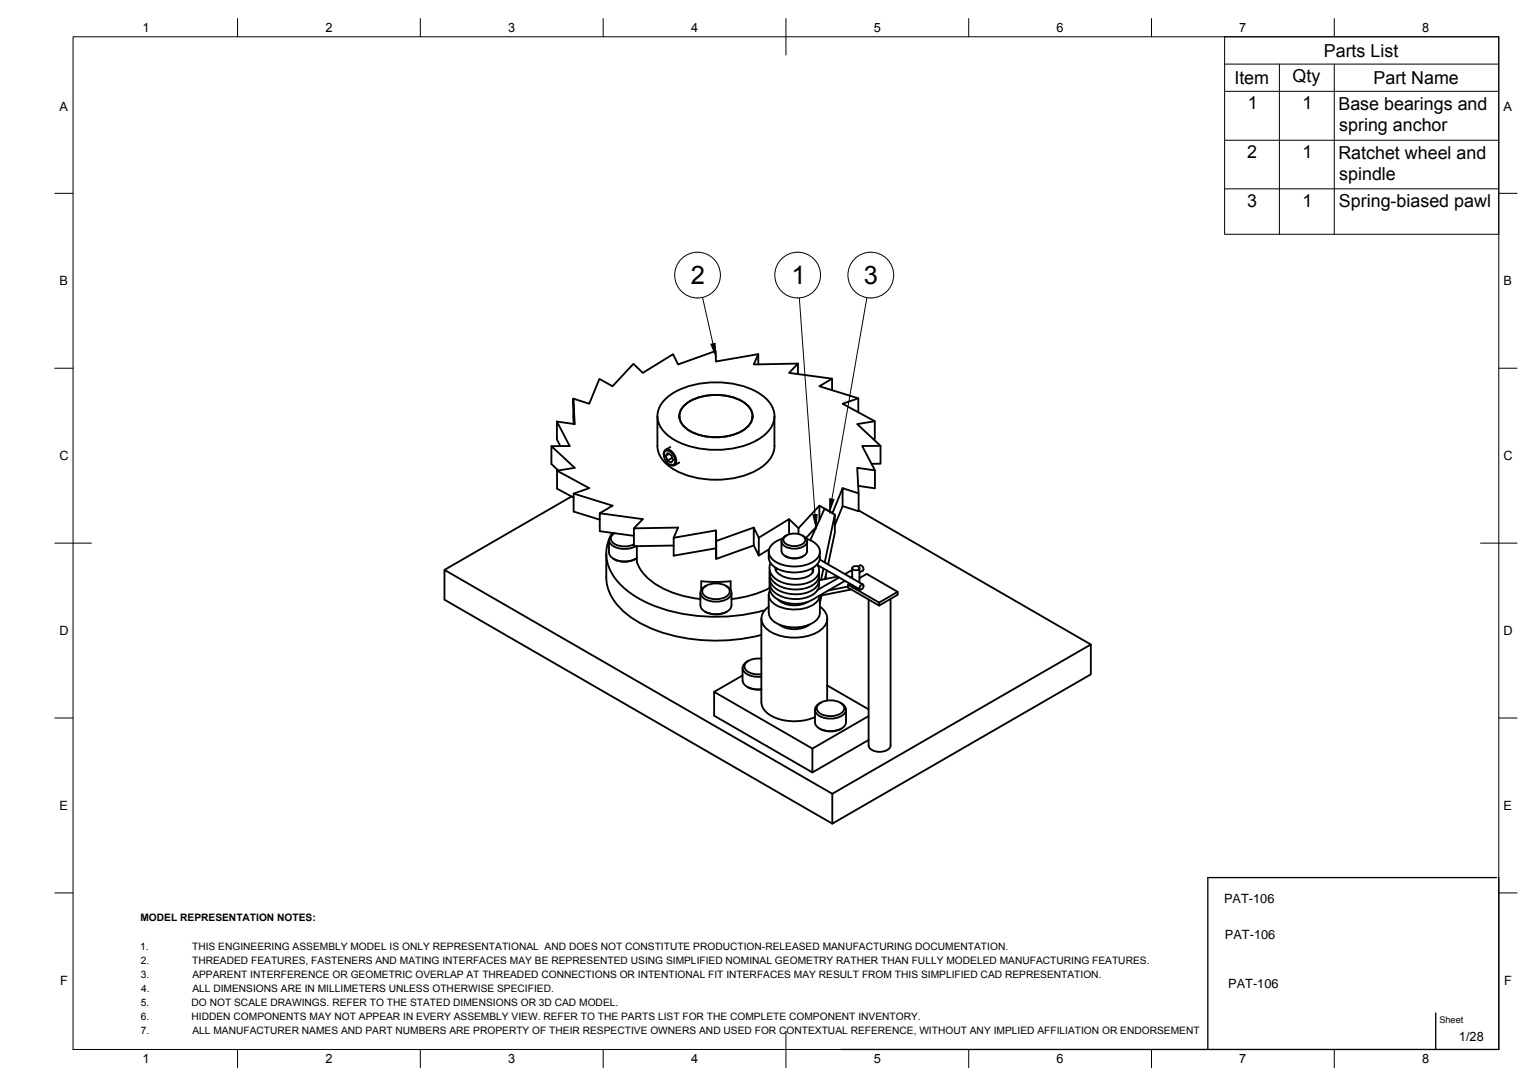
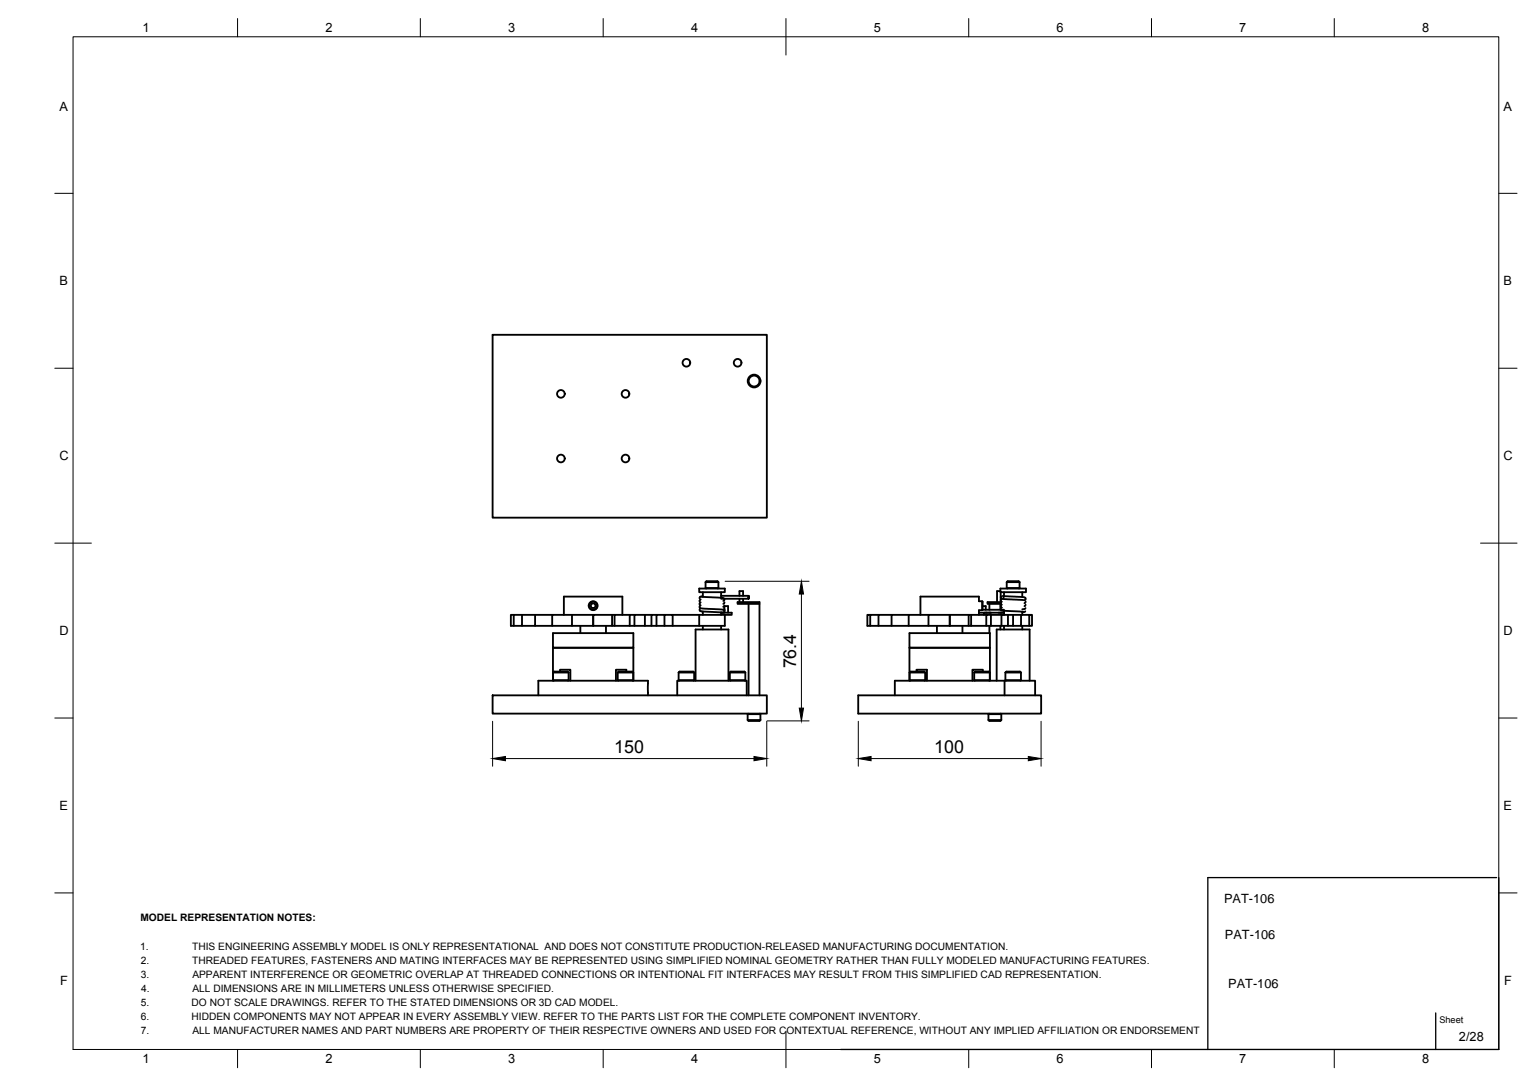
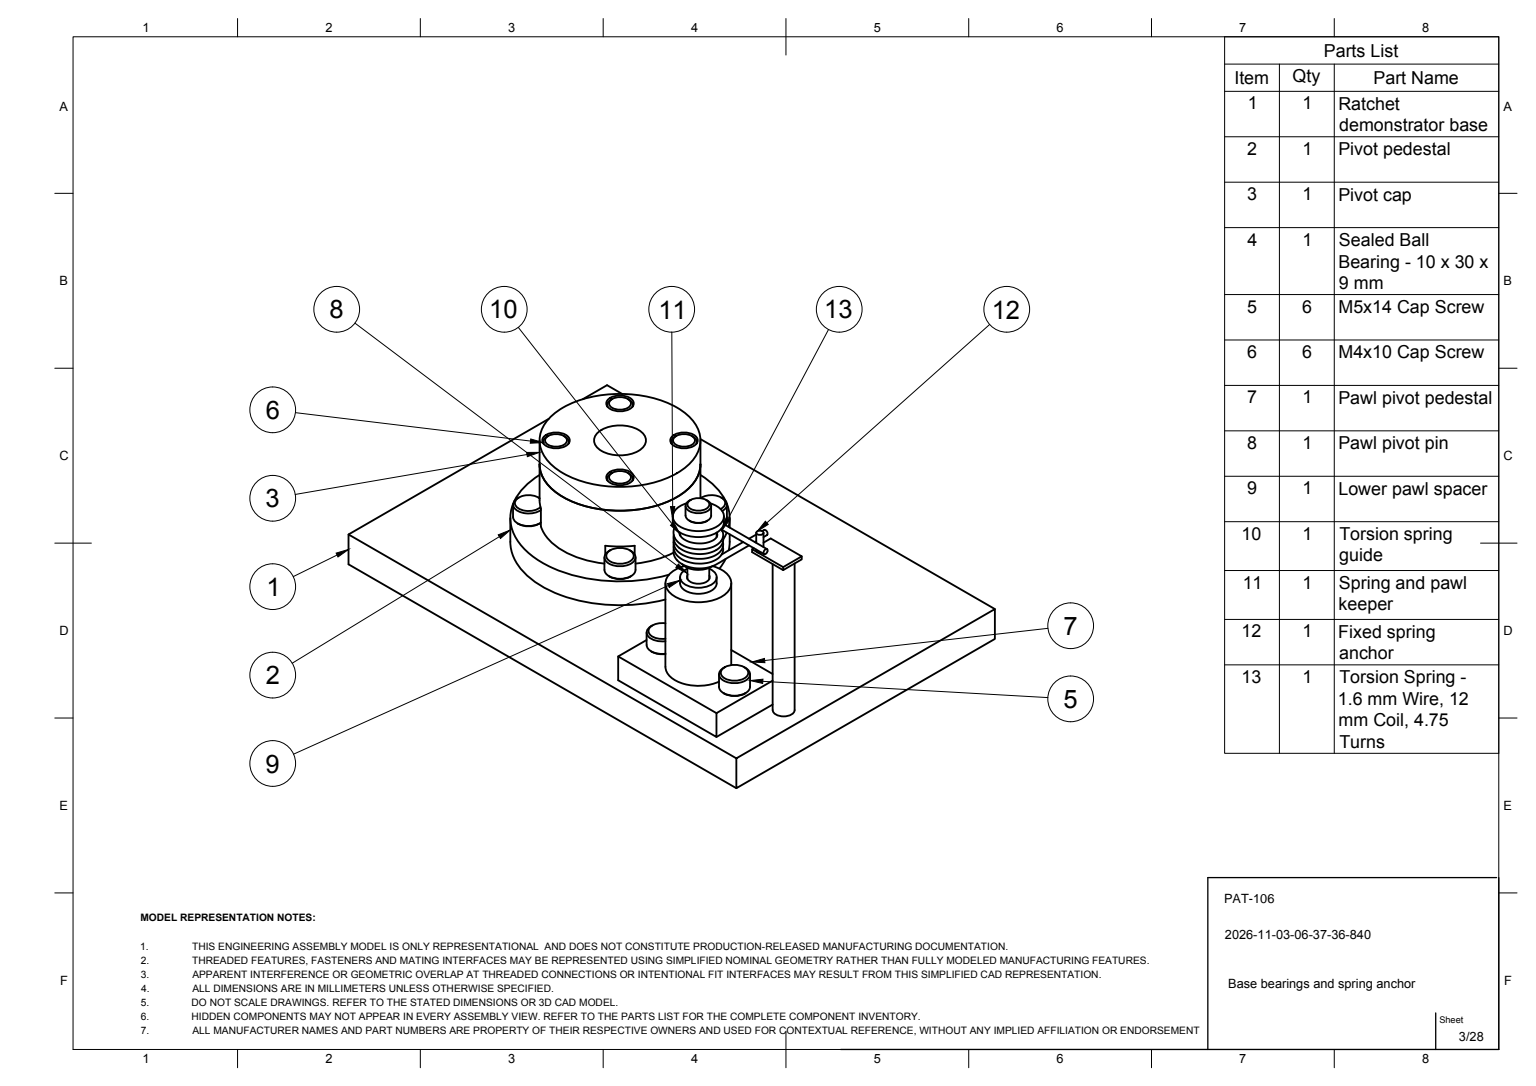
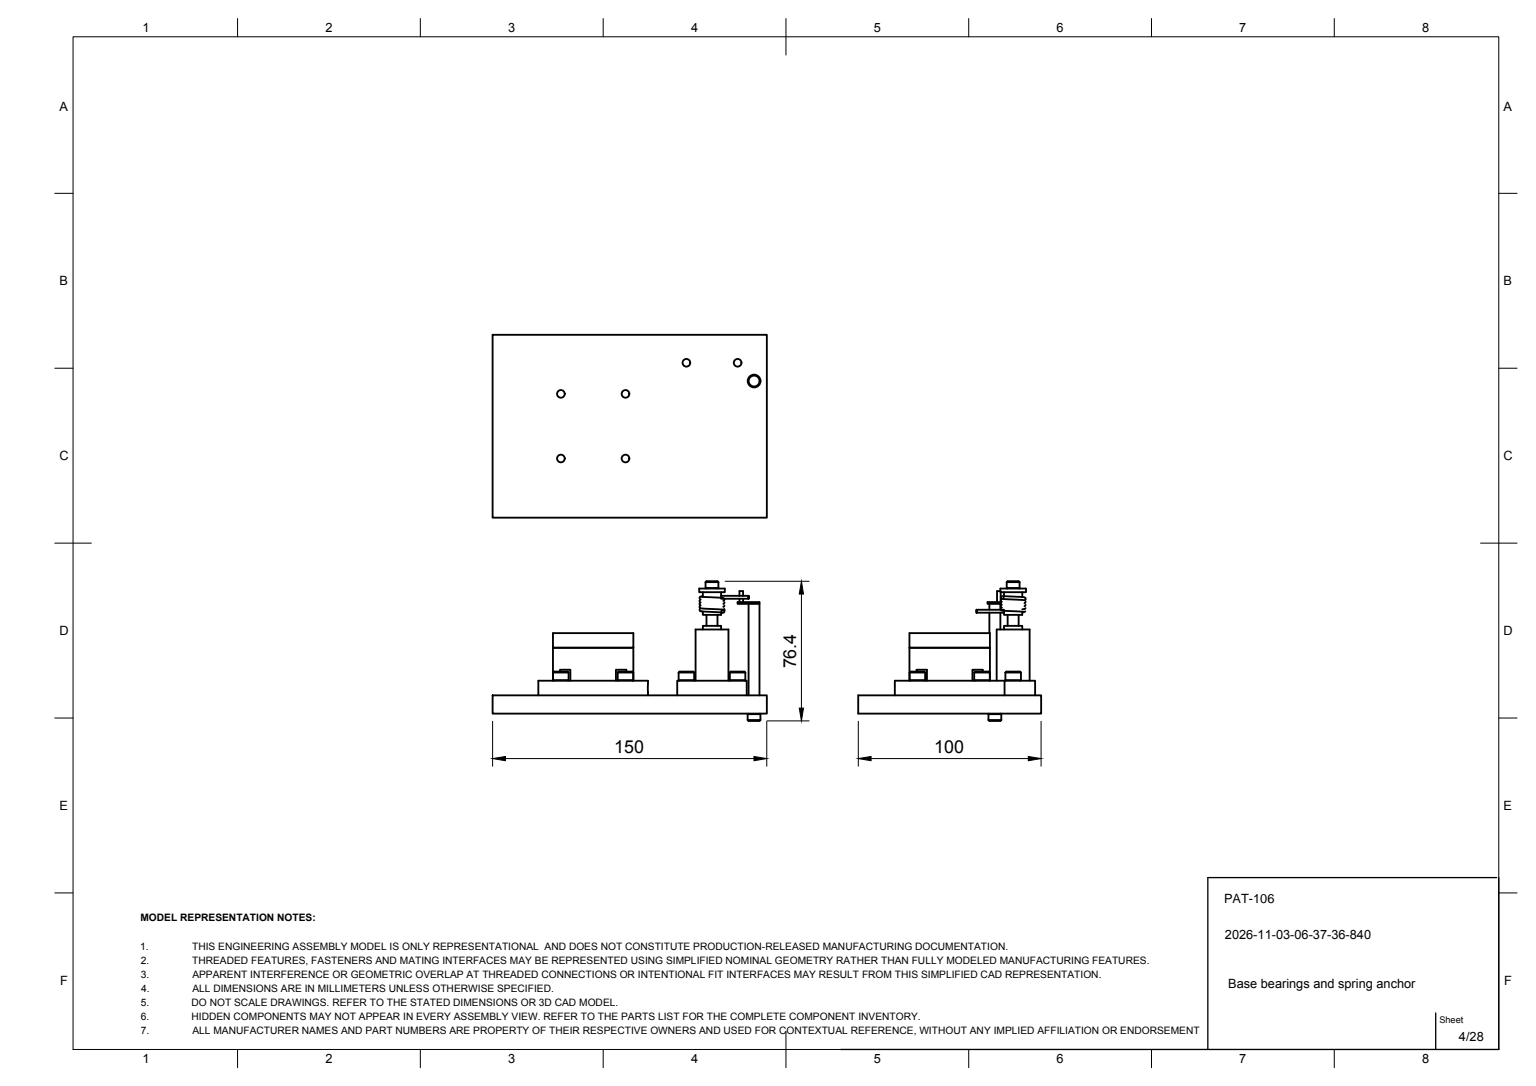
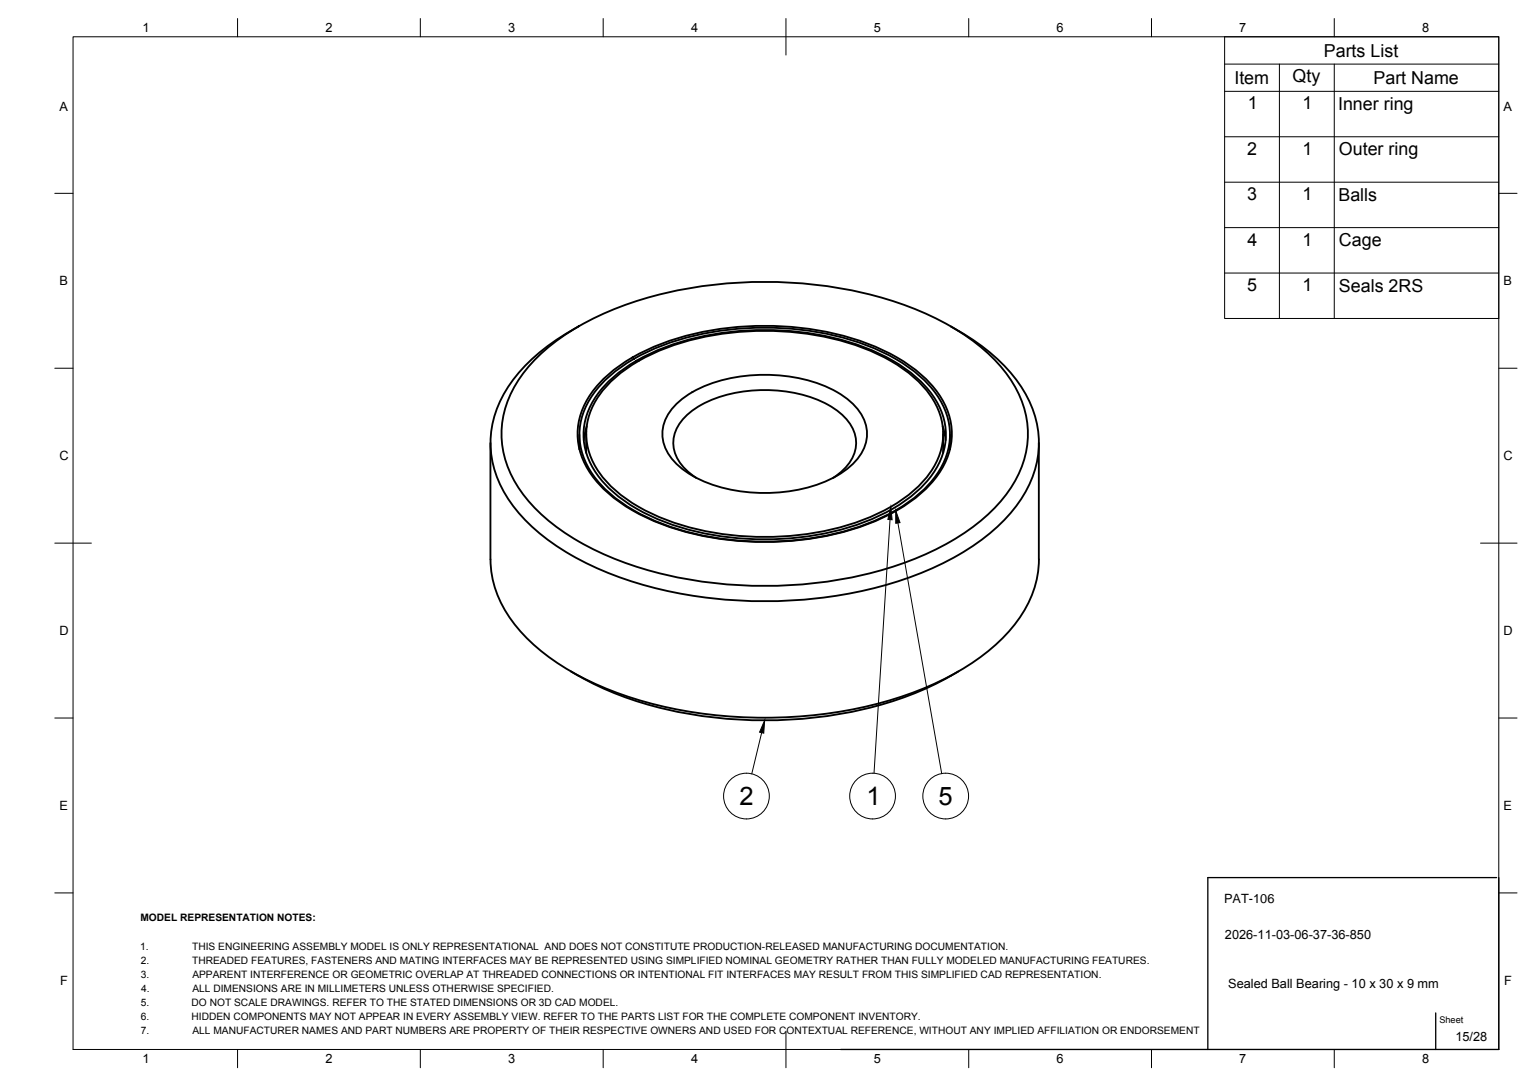
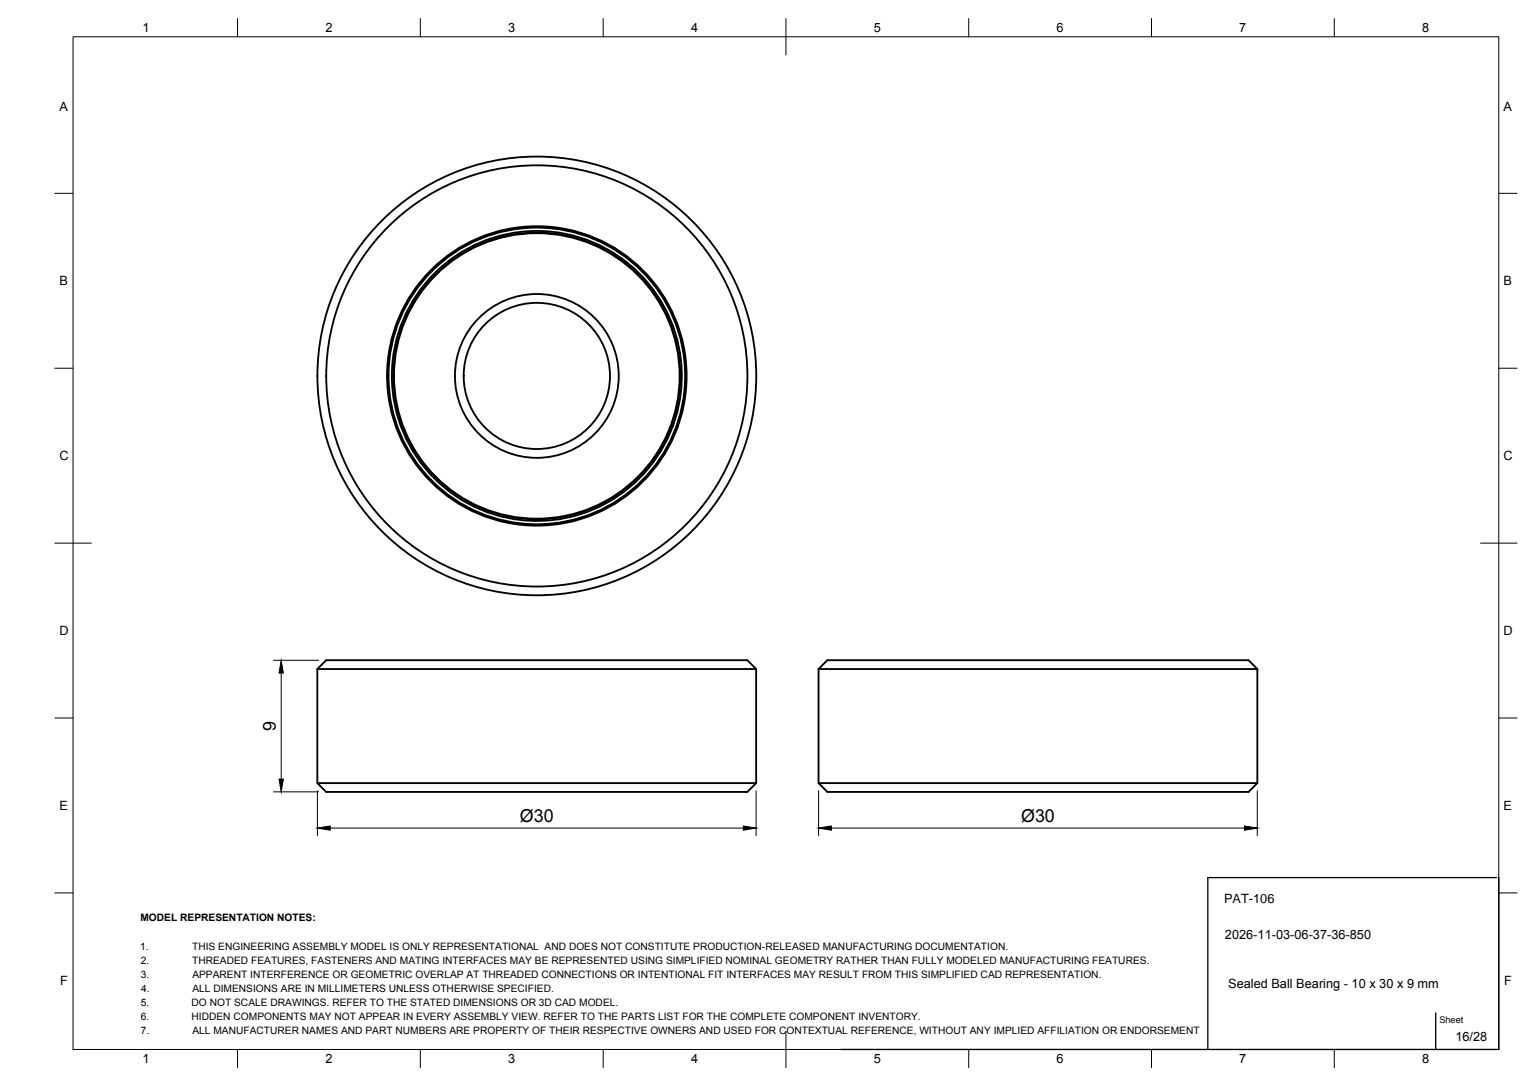
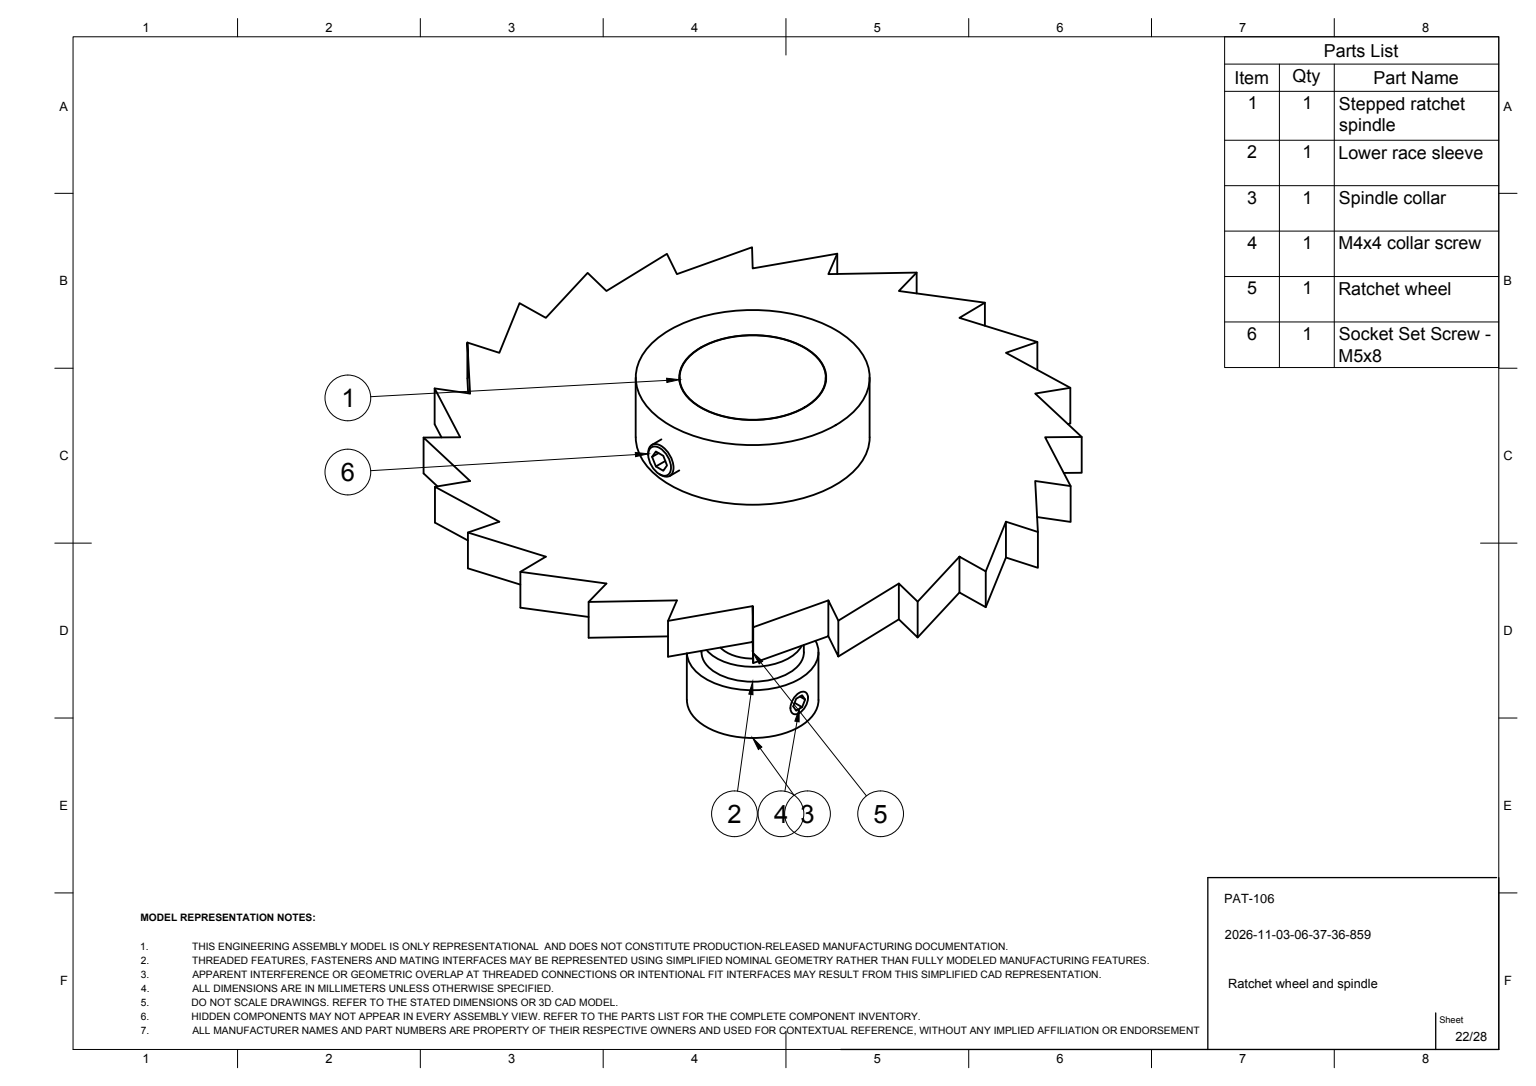
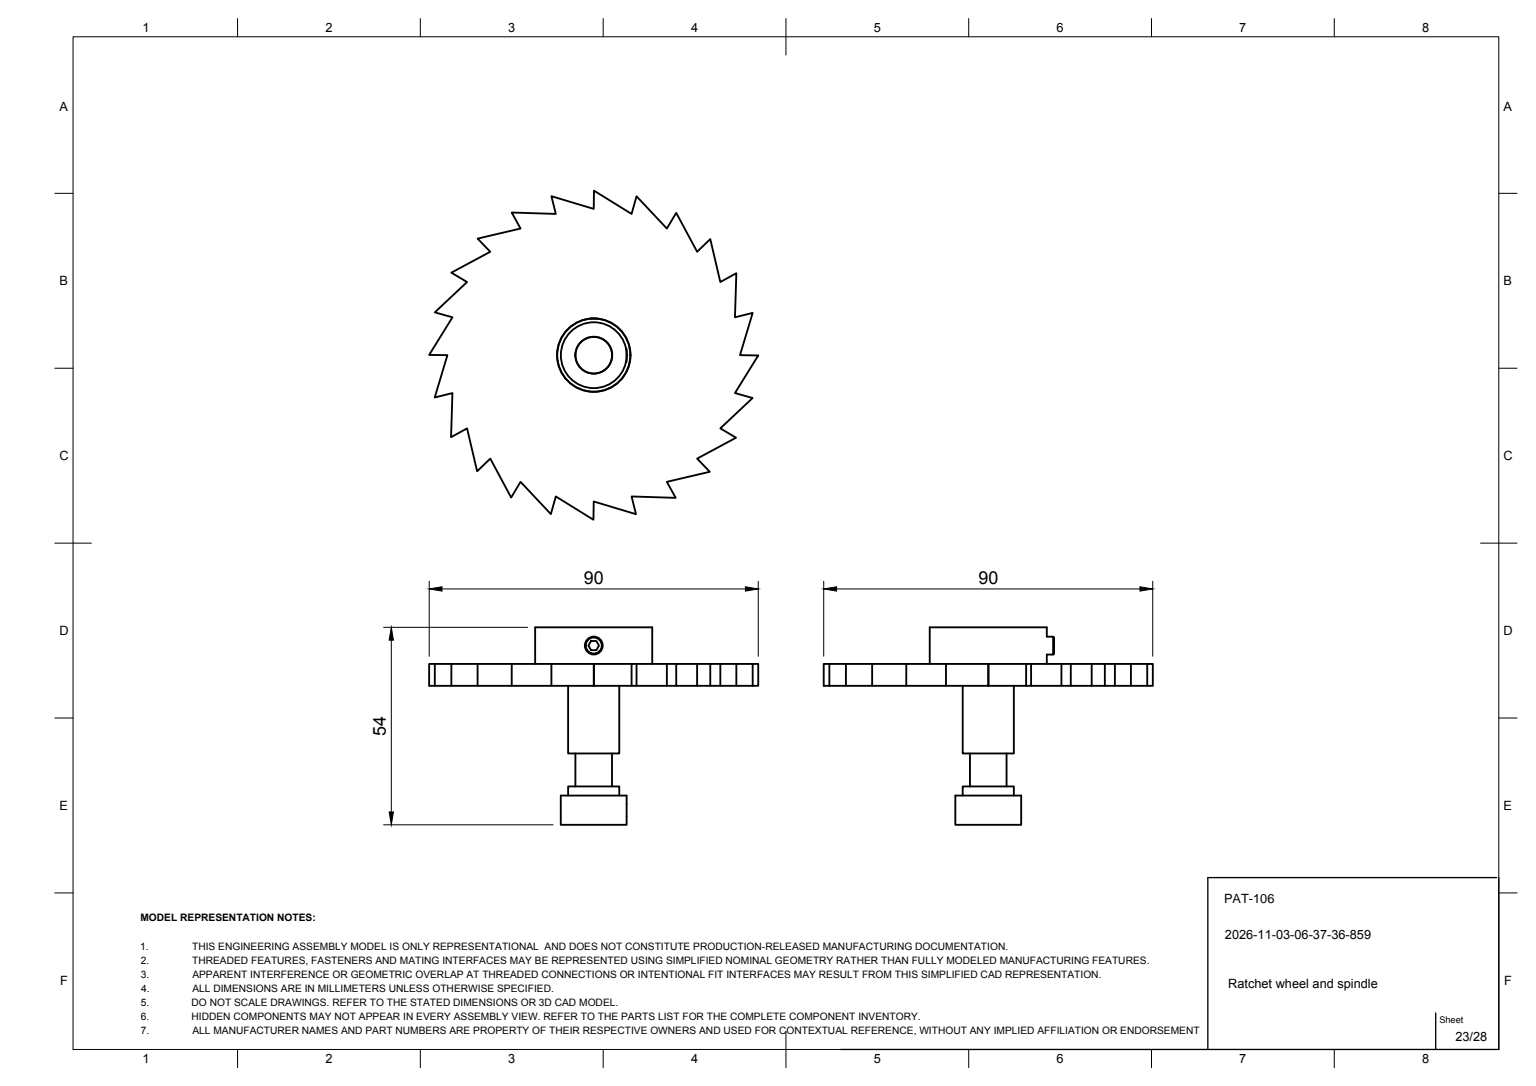
ISO-10303-21;
HEADER;
/* Generated by software containing ST-Developer
 * from STEP Tools, Inc. (www.steptools.com) 
 */

FILE_DESCRIPTION(
/* description */ ('Torsion-spring ratchet demonstrator'),
/* implementation_level */ '2;1');

FILE_NAME(
/* name */ 'PAT-106',
/* time_stamp */ '2026-10-29T17:29:17-07:00',
/* author */ (''),
/* organization */ (''),
/* preprocessor_version */ 'ST-DEVELOPER v20.2',
/* originating_system */ 'Autodesk Translation Framework v15.17.0.0',
/* authorisation */ '');

FILE_SCHEMA (('AUTOMOTIVE_DESIGN { 1 0 10303 214 3 1 1 }'));
ENDSEC;

DATA;
#10=MECHANICAL_DESIGN_GEOMETRIC_PRESENTATION_REPRESENTATION('',(#283,#284,
#285,#286,#287,#288,#289,#290,#291,#292,#293,#294,#295,#296,#297,#298,#299,
#300,#301,#302,#303,#304,#305,#306,#307,#308,#309,#310,#311,#312,#313,#314),
#11258);
#11=B_SPLINE_SURFACE_WITH_KNOTS('',3,3,((#8927,#8928,#8929,#8930,#8931,
#8932,#8933,#8934,#8935,#8936,#8937,#8938,#8939,#8940,#8941,#8942,#8943,
#8944,#8945,#8946,#8947,#8948,#8949,#8950,#8951,#8952,#8953,#8954,#8955,
#8956,#8957,#8958,#8959,#8960,#8961,#8962,#8963,#8964,#8965,#8966,#8967,
#8968,#8969,#8970,#8971,#8972,#8973,#8974,#8975,#8976,#8977,#8978,#8979,
#8980,#8981,#8982,#8983,#8984,#8985,#8986,#8987,#8988,#8989,#8990,#8991,
#8992,#8993),(#8994,#8995,#8996,#8997,#8998,#8999,#9000,#9001,#9002,#9003,
#9004,#9005,#9006,#9007,#9008,#9009,#9010,#9011,#9012,#9013,#9014,#9015,
#9016,#9017,#9018,#9019,#9020,#9021,#9022,#9023,#9024,#9025,#9026,#9027,
#9028,#9029,#9030,#9031,#9032,#9033,#9034,#9035,#9036,#9037,#9038,#9039,
#9040,#9041,#9042,#9043,#9044,#9045,#9046,#9047,#9048,#9049,#9050,#9051,
#9052,#9053,#9054,#9055,#9056,#9057,#9058,#9059,#9060),(#9061,#9062,#9063,
#9064,#9065,#9066,#9067,#9068,#9069,#9070,#9071,#9072,#9073,#9074,#9075,
#9076,#9077,#9078,#9079,#9080,#9081,#9082,#9083,#9084,#9085,#9086,#9087,
#9088,#9089,#9090,#9091,#9092,#9093,#9094,#9095,#9096,#9097,#9098,#9099,
#9100,#9101,#9102,#9103,#9104,#9105,#9106,#9107,#9108,#9109,#9110,#9111,
#9112,#9113,#9114,#9115,#9116,#9117,#9118,#9119,#9120,#9121,#9122,#9123,
#9124,#9125,#9126,#9127),(#9128,#9129,#9130,#9131,#9132,#9133,#9134,#9135,
#9136,#9137,#9138,#9139,#9140,#9141,#9142,#9143,#9144,#9145,#9146,#9147,
#9148,#9149,#9150,#9151,#9152,#9153,#9154,#9155,#9156,#9157,#9158,#9159,
#9160,#9161,#9162,#9163,#9164,#9165,#9166,#9167,#9168,#9169,#9170,#9171,
#9172,#9173,#9174,#9175,#9176,#9177,#9178,#9179,#9180,#9181,#9182,#9183,
#9184,#9185,#9186,#9187,#9188,#9189,#9190,#9191,#9192,#9193,#9194),(#9195,
#9196,#9197,#9198,#9199,#9200,#9201,#9202,#9203,#9204,#9205,#9206,#9207,
#9208,#9209,#9210,#9211,#9212,#9213,#9214,#9215,#9216,#9217,#9218,#9219,
#9220,#9221,#9222,#9223,#9224,#9225,#9226,#9227,#9228,#9229,#9230,#9231,
#9232,#9233,#9234,#9235,#9236,#9237,#9238,#9239,#9240,#9241,#9242,#9243,
#9244,#9245,#9246,#9247,#9248,#9249,#9250,#9251,#9252,#9253,#9254,#9255,
#9256,#9257,#9258,#9259,#9260,#9261),(#9262,#9263,#9264,#9265,#9266,#9267,
#9268,#9269,#9270,#9271,#9272,#9273,#9274,#9275,#9276,#9277,#9278,#9279,
#9280,#9281,#9282,#9283,#9284,#9285,#9286,#9287,#9288,#9289,#9290,#9291,
#9292,#9293,#9294,#9295,#9296,#9297,#9298,#9299,#9300,#9301,#9302,#9303,
#9304,#9305,#9306,#9307,#9308,#9309,#9310,#9311,#9312,#9313,#9314,#9315,
#9316,#9317,#9318,#9319,#9320,#9321,#9322,#9323,#9324,#9325,#9326,#9327,
#9328),(#9329,#9330,#9331,#9332,#9333,#9334,#9335,#9336,#9337,#9338,#9339,
#9340,#9341,#9342,#9343,#9344,#9345,#9346,#9347,#9348,#9349,#9350,#9351,
#9352,#9353,#9354,#9355,#9356,#9357,#9358,#9359,#9360,#9361,#9362,#9363,
#9364,#9365,#9366,#9367,#9368,#9369,#9370,#9371,#9372,#9373,#9374,#9375,
#9376,#9377,#9378,#9379,#9380,#9381,#9382,#9383,#9384,#9385,#9386,#9387,
#9388,#9389,#9390,#9391,#9392,#9393,#9394,#9395),(#9396,#9397,#9398,#9399,
#9400,#9401,#9402,#9403,#9404,#9405,#9406,#9407,#9408,#9409,#9410,#9411,
#9412,#9413,#9414,#9415,#9416,#9417,#9418,#9419,#9420,#9421,#9422,#9423,
#9424,#9425,#9426,#9427,#9428,#9429,#9430,#9431,#9432,#9433,#9434,#9435,
#9436,#9437,#9438,#9439,#9440,#9441,#9442,#9443,#9444,#9445,#9446,#9447,
#9448,#9449,#9450,#9451,#9452,#9453,#9454,#9455,#9456,#9457,#9458,#9459,
#9460,#9461,#9462),(#9463,#9464,#9465,#9466,#9467,#9468,#9469,#9470,#9471,
#9472,#9473,#9474,#9475,#9476,#9477,#9478,#9479,#9480,#9481,#9482,#9483,
#9484,#9485,#9486,#9487,#9488,#9489,#9490,#9491,#9492,#9493,#9494,#9495,
#9496,#9497,#9498,#9499,#9500,#9501,#9502,#9503,#9504,#9505,#9506,#9507,
#9508,#9509,#9510,#9511,#9512,#9513,#9514,#9515,#9516,#9517,#9518,#9519,
#9520,#9521,#9522,#9523,#9524,#9525,#9526,#9527,#9528,#9529)),
 .UNSPECIFIED.,.F.,.F.,.F.,(4,1,1,1,1,1,4),(4,1,1,1,1,1,1,1,1,1,1,1,1,1,
1,1,1,1,1,1,1,1,1,1,1,1,1,1,1,1,1,1,1,1,1,1,1,1,1,1,1,1,1,1,1,1,1,1,1,1,
1,1,1,1,1,1,1,1,1,1,1,1,1,1,4),(-2.2472005777546,-1.52802098913967,-0.808841400524738,
-0.329388341448117,0.150064717628504,0.629517776705124,1.10897083578174),
(0.,0.0178571428571429,0.0357142857142857,0.0446428571428571,0.0535714285714286,
0.0625,0.0714285714285714,0.0803571428571428,0.0848214285714286,0.0892857142857143,
0.0982142857142857,0.107142857142857,0.125,0.142857142857143,0.166666666666667,
0.19047619047619,0.214285714285714,0.232142857142857,0.25,0.267857142857143,
0.285714285714286,0.303571428571429,0.321428571428571,0.339285714285714,
0.357142857142857,0.369047619047619,0.392857142857143,0.410714285714286,
0.428571428571429,0.452380952380952,0.476190476190476,0.492063492063492,
0.507936507936508,0.523809523809524,0.547619047619048,0.571428571428571,
0.595238095238095,0.619047619047619,0.642857142857143,0.666666666666667,
0.682539682539682,0.698412698412698,0.714285714285714,0.73015873015873,
0.746031746031746,0.761904761904762,0.785714285714286,0.809523809523809,
0.833333333333333,0.857142857142857,0.861607142857143,0.866071428571429,
0.875,0.892857142857143,0.901785714285714,0.910714285714286,0.915178571428571,
0.919642857142857,0.928571428571429,0.9375,0.946428571428571,0.955357142857143,
0.964285714285714,0.982142857142857,1.),.UNSPECIFIED.);
#12=B_SPLINE_SURFACE_WITH_KNOTS('',3,3,((#9670,#9671,#9672,#9673,#9674,
#9675,#9676,#9677,#9678,#9679,#9680,#9681,#9682,#9683,#9684,#9685,#9686,
#9687,#9688,#9689,#9690,#9691,#9692,#9693,#9694,#9695,#9696,#9697,#9698,
#9699,#9700,#9701,#9702,#9703,#9704,#9705,#9706,#9707,#9708,#9709,#9710,
#9711,#9712,#9713,#9714,#9715,#9716,#9717,#9718,#9719,#9720,#9721,#9722,
#9723,#9724,#9725,#9726,#9727,#9728,#9729,#9730,#9731,#9732,#9733,#9734,
#9735,#9736,#9737,#9738,#9739,#9740),(#9741,#9742,#9743,#9744,#9745,#9746,
#9747,#9748,#9749,#9750,#9751,#9752,#9753,#9754,#9755,#9756,#9757,#9758,
#9759,#9760,#9761,#9762,#9763,#9764,#9765,#9766,#9767,#9768,#9769,#9770,
#9771,#9772,#9773,#9774,#9775,#9776,#9777,#9778,#9779,#9780,#9781,#9782,
#9783,#9784,#9785,#9786,#9787,#9788,#9789,#9790,#9791,#9792,#9793,#9794,
#9795,#9796,#9797,#9798,#9799,#9800,#9801,#9802,#9803,#9804,#9805,#9806,
#9807,#9808,#9809,#9810,#9811),(#9812,#9813,#9814,#9815,#9816,#9817,#9818,
#9819,#9820,#9821,#9822,#9823,#9824,#9825,#9826,#9827,#9828,#9829,#9830,
#9831,#9832,#9833,#9834,#9835,#9836,#9837,#9838,#9839,#9840,#9841,#9842,
#9843,#9844,#9845,#9846,#9847,#9848,#9849,#9850,#9851,#9852,#9853,#9854,
#9855,#9856,#9857,#9858,#9859,#9860,#9861,#9862,#9863,#9864,#9865,#9866,
#9867,#9868,#9869,#9870,#9871,#9872,#9873,#9874,#9875,#9876,#9877,#9878,
#9879,#9880,#9881,#9882),(#9883,#9884,#9885,#9886,#9887,#9888,#9889,#9890,
#9891,#9892,#9893,#9894,#9895,#9896,#9897,#9898,#9899,#9900,#9901,#9902,
#9903,#9904,#9905,#9906,#9907,#9908,#9909,#9910,#9911,#9912,#9913,#9914,
#9915,#9916,#9917,#9918,#9919,#9920,#9921,#9922,#9923,#9924,#9925,#9926,
#9927,#9928,#9929,#9930,#9931,#9932,#9933,#9934,#9935,#9936,#9937,#9938,
#9939,#9940,#9941,#9942,#9943,#9944,#9945,#9946,#9947,#9948,#9949,#9950,
#9951,#9952,#9953)),.UNSPECIFIED.,.F.,.F.,.F.,(4,4),(4,1,1,1,1,1,1,1,1,
1,1,1,1,1,1,1,1,1,1,1,1,1,1,1,1,1,1,1,1,1,1,1,1,1,1,1,1,1,1,1,1,1,1,1,1,
1,1,1,1,1,1,1,1,1,1,1,1,1,1,1,1,1,1,1,1,1,1,1,4),(3.14159265358979,4.03598472942499),
(0.,0.0178571428571429,0.0357142857142857,0.0446428571428571,0.0535714285714286,
0.0625,0.0714285714285714,0.0803571428571428,0.0892857142857143,0.0982142857142857,
0.107142857142857,0.125,0.142857142857143,0.166666666666667,0.19047619047619,
0.196428571428571,0.214285714285714,0.232142857142857,0.25,0.267857142857143,
0.285714285714286,0.303571428571429,0.321428571428571,0.339285714285714,
0.357142857142857,0.369047619047619,0.392857142857143,0.410714285714286,
0.419642857142857,0.428571428571429,0.452380952380952,0.476190476190476,
0.492063492063492,0.5,0.507936507936508,0.523809523809524,0.547619047619048,
0.571428571428571,0.595238095238095,0.619047619047619,0.642857142857143,
0.666666666666667,0.682539682539682,0.698412698412698,0.714285714285714,
0.722222222222222,0.73015873015873,0.746031746031746,0.761904761904762,
0.773809523809524,0.785714285714286,0.809523809523809,0.833333333333333,
0.857142857142857,0.859375,0.861607142857143,0.866071428571429,0.875,0.892857142857143,
0.901785714285714,0.910714285714286,0.919642857142857,0.928571428571429,
0.9375,0.946428571428571,0.955357142857143,0.964285714285714,0.982142857142857,
1.),.UNSPECIFIED.);
#13=B_SPLINE_SURFACE_WITH_KNOTS('',3,3,((#10029,#10030,#10031,#10032,#10033,
#10034,#10035,#10036,#10037,#10038,#10039,#10040,#10041,#10042,#10043,#10044,
#10045,#10046,#10047,#10048,#10049,#10050,#10051,#10052,#10053,#10054,#10055,
#10056,#10057,#10058,#10059,#10060,#10061,#10062,#10063,#10064,#10065,#10066,
#10067,#10068,#10069,#10070,#10071,#10072,#10073,#10074,#10075,#10076,#10077,
#10078,#10079,#10080,#10081,#10082,#10083,#10084,#10085,#10086,#10087,#10088,
#10089,#10090,#10091,#10092,#10093,#10094,#10095,#10096,#10097,#10098,#10099,
#10100),(#10101,#10102,#10103,#10104,#10105,#10106,#10107,#10108,#10109,
#10110,#10111,#10112,#10113,#10114,#10115,#10116,#10117,#10118,#10119,#10120,
#10121,#10122,#10123,#10124,#10125,#10126,#10127,#10128,#10129,#10130,#10131,
#10132,#10133,#10134,#10135,#10136,#10137,#10138,#10139,#10140,#10141,#10142,
#10143,#10144,#10145,#10146,#10147,#10148,#10149,#10150,#10151,#10152,#10153,
#10154,#10155,#10156,#10157,#10158,#10159,#10160,#10161,#10162,#10163,#10164,
#10165,#10166,#10167,#10168,#10169,#10170,#10171,#10172),(#10173,#10174,
#10175,#10176,#10177,#10178,#10179,#10180,#10181,#10182,#10183,#10184,#10185,
#10186,#10187,#10188,#10189,#10190,#10191,#10192,#10193,#10194,#10195,#10196,
#10197,#10198,#10199,#10200,#10201,#10202,#10203,#10204,#10205,#10206,#10207,
#10208,#10209,#10210,#10211,#10212,#10213,#10214,#10215,#10216,#10217,#10218,
#10219,#10220,#10221,#10222,#10223,#10224,#10225,#10226,#10227,#10228,#10229,
#10230,#10231,#10232,#10233,#10234,#10235,#10236,#10237,#10238,#10239,#10240,
#10241,#10242,#10243,#10244),(#10245,#10246,#10247,#10248,#10249,#10250,
#10251,#10252,#10253,#10254,#10255,#10256,#10257,#10258,#10259,#10260,#10261,
#10262,#10263,#10264,#10265,#10266,#10267,#10268,#10269,#10270,#10271,#10272,
#10273,#10274,#10275,#10276,#10277,#10278,#10279,#10280,#10281,#10282,#10283,
#10284,#10285,#10286,#10287,#10288,#10289,#10290,#10291,#10292,#10293,#10294,
#10295,#10296,#10297,#10298,#10299,#10300,#10301,#10302,#10303,#10304,#10305,
#10306,#10307,#10308,#10309,#10310,#10311,#10312,#10313,#10314,#10315,#10316),
(#10317,#10318,#10319,#10320,#10321,#10322,#10323,#10324,#10325,#10326,
#10327,#10328,#10329,#10330,#10331,#10332,#10333,#10334,#10335,#10336,#10337,
#10338,#10339,#10340,#10341,#10342,#10343,#10344,#10345,#10346,#10347,#10348,
#10349,#10350,#10351,#10352,#10353,#10354,#10355,#10356,#10357,#10358,#10359,
#10360,#10361,#10362,#10363,#10364,#10365,#10366,#10367,#10368,#10369,#10370,
#10371,#10372,#10373,#10374,#10375,#10376,#10377,#10378,#10379,#10380,#10381,
#10382,#10383,#10384,#10385,#10386,#10387,#10388),(#10389,#10390,#10391,
#10392,#10393,#10394,#10395,#10396,#10397,#10398,#10399,#10400,#10401,#10402,
#10403,#10404,#10405,#10406,#10407,#10408,#10409,#10410,#10411,#10412,#10413,
#10414,#10415,#10416,#10417,#10418,#10419,#10420,#10421,#10422,#10423,#10424,
#10425,#10426,#10427,#10428,#10429,#10430,#10431,#10432,#10433,#10434,#10435,
#10436,#10437,#10438,#10439,#10440,#10441,#10442,#10443,#10444,#10445,#10446,
#10447,#10448,#10449,#10450,#10451,#10452,#10453,#10454,#10455,#10456,#10457,
#10458,#10459,#10460)),.UNSPECIFIED.,.F.,.F.,.F.,(4,1,1,4),(4,1,1,1,1,1,
1,1,1,1,1,1,1,1,1,1,1,1,1,1,1,1,1,1,1,1,1,1,1,1,1,1,1,1,1,1,1,1,1,1,1,1,
1,1,1,1,1,1,1,1,1,1,1,1,1,1,1,1,1,1,1,1,1,1,1,1,1,1,1,4),(1.10897083578174,
1.98009447198525,2.56084356278759,3.14159265358993),(0.,0.0178571428571429,
0.0357142857142857,0.0446428571428571,0.0535714285714286,0.0625,0.0714285714285714,
0.0803571428571428,0.0848214285714286,0.0892857142857143,0.0982142857142857,
0.107142857142857,0.125,0.142857142857143,0.166666666666667,0.19047619047619,
0.196428571428571,0.214285714285714,0.232142857142857,0.25,0.267857142857143,
0.285714285714286,0.303571428571429,0.321428571428571,0.339285714285714,
0.357142857142857,0.369047619047619,0.392857142857143,0.410714285714286,
0.419642857142857,0.428571428571429,0.452380952380952,0.476190476190476,
0.492063492063492,0.507936507936508,0.523809523809524,0.547619047619048,
0.571428571428571,0.595238095238095,0.619047619047619,0.642857142857143,
0.666666666666667,0.682539682539682,0.698412698412698,0.714285714285714,
0.73015873015873,0.746031746031746,0.761904761904762,0.773809523809524,
0.785714285714286,0.791666666666667,0.809523809523809,0.833333333333333,
0.857142857142857,0.859375,0.861607142857143,0.866071428571429,0.875,0.892857142857143,
0.901785714285714,0.910714285714286,0.915178571428571,0.919642857142857,
0.928571428571429,0.9375,0.946428571428571,0.955357142857143,0.964285714285714,
0.982142857142857,1.),.UNSPECIFIED.);
#14=ORIENTED_CLOSED_SHELL('',*,#5176,.F.);
#15=ORIENTED_CLOSED_SHELL('',*,#5178,.F.);
#16=BREP_WITH_VOIDS('Body1',#5177,(#14));
#17=BREP_WITH_VOIDS('Body1',#5179,(#15));
#18=ITEM_DEFINED_TRANSFORMATION($,$,#5681,#5809);
#19=ITEM_DEFINED_TRANSFORMATION($,$,#5701,#5810);
#20=ITEM_DEFINED_TRANSFORMATION($,$,#5721,#5811);
#21=ITEM_DEFINED_TRANSFORMATION($,$,#5738,#5812);
#22=ITEM_DEFINED_TRANSFORMATION($,$,#5792,#5813);
#23=ITEM_DEFINED_TRANSFORMATION($,$,#5455,#5871);
#24=ITEM_DEFINED_TRANSFORMATION($,$,#5483,#5872);
#25=ITEM_DEFINED_TRANSFORMATION($,$,#5507,#5873);
#26=ITEM_DEFINED_TRANSFORMATION($,$,#5521,#5874);
#27=ITEM_DEFINED_TRANSFORMATION($,$,#5530,#5875);
#28=ITEM_DEFINED_TRANSFORMATION($,$,#5539,#5876);
#29=ITEM_DEFINED_TRANSFORMATION($,$,#5548,#5877);
#30=ITEM_DEFINED_TRANSFORMATION($,$,#5569,#5878);
#31=ITEM_DEFINED_TRANSFORMATION($,$,#5639,#5879);
#32=ITEM_DEFINED_TRANSFORMATION($,$,#5680,#5880);
#33=ITEM_DEFINED_TRANSFORMATION($,$,#5814,#5881);
#34=ITEM_DEFINED_TRANSFORMATION($,$,#5838,#5882);
#35=ITEM_DEFINED_TRANSFORMATION($,$,#5814,#5883);
#36=ITEM_DEFINED_TRANSFORMATION($,$,#5838,#5884);
#37=ITEM_DEFINED_TRANSFORMATION($,$,#5814,#5885);
#38=ITEM_DEFINED_TRANSFORMATION($,$,#5838,#5886);
#39=ITEM_DEFINED_TRANSFORMATION($,$,#5814,#5887);
#40=ITEM_DEFINED_TRANSFORMATION($,$,#5838,#5888);
#41=ITEM_DEFINED_TRANSFORMATION($,$,#5814,#5889);
#42=ITEM_DEFINED_TRANSFORMATION($,$,#5814,#5890);
#43=ITEM_DEFINED_TRANSFORMATION($,$,#5838,#5891);
#44=ITEM_DEFINED_TRANSFORMATION($,$,#5838,#5892);
#45=ITEM_DEFINED_TRANSFORMATION($,$,#5862,#5893);
#46=ITEM_DEFINED_TRANSFORMATION($,$,#5895,#6028);
#47=ITEM_DEFINED_TRANSFORMATION($,$,#5909,#6029);
#48=ITEM_DEFINED_TRANSFORMATION($,$,#5918,#6030);
#49=ITEM_DEFINED_TRANSFORMATION($,$,#5932,#6031);
#50=ITEM_DEFINED_TRANSFORMATION($,$,#5947,#6032);
#51=ITEM_DEFINED_TRANSFORMATION($,$,#6011,#6033);
#52=ITEM_DEFINED_TRANSFORMATION($,$,#6035,#6062);
#53=ITEM_DEFINED_TRANSFORMATION($,$,#5454,#6063);
#54=ITEM_DEFINED_TRANSFORMATION($,$,#5894,#6064);
#55=ITEM_DEFINED_TRANSFORMATION($,$,#6034,#6065);
#56=(
REPRESENTATION_RELATIONSHIP($,$,#11371,#11370)
REPRESENTATION_RELATIONSHIP_WITH_TRANSFORMATION(#18)
SHAPE_REPRESENTATION_RELATIONSHIP()
);
#57=(
REPRESENTATION_RELATIONSHIP($,$,#11372,#11370)
REPRESENTATION_RELATIONSHIP_WITH_TRANSFORMATION(#19)
SHAPE_REPRESENTATION_RELATIONSHIP()
);
#58=(
REPRESENTATION_RELATIONSHIP($,$,#11373,#11370)
REPRESENTATION_RELATIONSHIP_WITH_TRANSFORMATION(#20)
SHAPE_REPRESENTATION_RELATIONSHIP()
);
#59=(
REPRESENTATION_RELATIONSHIP($,$,#11374,#11370)
REPRESENTATION_RELATIONSHIP_WITH_TRANSFORMATION(#21)
SHAPE_REPRESENTATION_RELATIONSHIP()
);
#60=(
REPRESENTATION_RELATIONSHIP($,$,#11375,#11370)
REPRESENTATION_RELATIONSHIP_WITH_TRANSFORMATION(#22)
SHAPE_REPRESENTATION_RELATIONSHIP()
);
#61=(
REPRESENTATION_RELATIONSHIP($,$,#11361,#11360)
REPRESENTATION_RELATIONSHIP_WITH_TRANSFORMATION(#23)
SHAPE_REPRESENTATION_RELATIONSHIP()
);
#62=(
REPRESENTATION_RELATIONSHIP($,$,#11362,#11360)
REPRESENTATION_RELATIONSHIP_WITH_TRANSFORMATION(#24)
SHAPE_REPRESENTATION_RELATIONSHIP()
);
#63=(
REPRESENTATION_RELATIONSHIP($,$,#11363,#11360)
REPRESENTATION_RELATIONSHIP_WITH_TRANSFORMATION(#25)
SHAPE_REPRESENTATION_RELATIONSHIP()
);
#64=(
REPRESENTATION_RELATIONSHIP($,$,#11364,#11360)
REPRESENTATION_RELATIONSHIP_WITH_TRANSFORMATION(#26)
SHAPE_REPRESENTATION_RELATIONSHIP()
);
#65=(
REPRESENTATION_RELATIONSHIP($,$,#11365,#11360)
REPRESENTATION_RELATIONSHIP_WITH_TRANSFORMATION(#27)
SHAPE_REPRESENTATION_RELATIONSHIP()
);
#66=(
REPRESENTATION_RELATIONSHIP($,$,#11366,#11360)
REPRESENTATION_RELATIONSHIP_WITH_TRANSFORMATION(#28)
SHAPE_REPRESENTATION_RELATIONSHIP()
);
#67=(
REPRESENTATION_RELATIONSHIP($,$,#11367,#11360)
REPRESENTATION_RELATIONSHIP_WITH_TRANSFORMATION(#29)
SHAPE_REPRESENTATION_RELATIONSHIP()
);
#68=(
REPRESENTATION_RELATIONSHIP($,$,#11368,#11360)
REPRESENTATION_RELATIONSHIP_WITH_TRANSFORMATION(#30)
SHAPE_REPRESENTATION_RELATIONSHIP()
);
#69=(
REPRESENTATION_RELATIONSHIP($,$,#11369,#11360)
REPRESENTATION_RELATIONSHIP_WITH_TRANSFORMATION(#31)
SHAPE_REPRESENTATION_RELATIONSHIP()
);
#70=(
REPRESENTATION_RELATIONSHIP($,$,#11370,#11360)
REPRESENTATION_RELATIONSHIP_WITH_TRANSFORMATION(#32)
SHAPE_REPRESENTATION_RELATIONSHIP()
);
#71=(
REPRESENTATION_RELATIONSHIP($,$,#11376,#11360)
REPRESENTATION_RELATIONSHIP_WITH_TRANSFORMATION(#33)
SHAPE_REPRESENTATION_RELATIONSHIP()
);
#72=(
REPRESENTATION_RELATIONSHIP($,$,#11377,#11360)
REPRESENTATION_RELATIONSHIP_WITH_TRANSFORMATION(#34)
SHAPE_REPRESENTATION_RELATIONSHIP()
);
#73=(
REPRESENTATION_RELATIONSHIP($,$,#11376,#11360)
REPRESENTATION_RELATIONSHIP_WITH_TRANSFORMATION(#35)
SHAPE_REPRESENTATION_RELATIONSHIP()
);
#74=(
REPRESENTATION_RELATIONSHIP($,$,#11377,#11360)
REPRESENTATION_RELATIONSHIP_WITH_TRANSFORMATION(#36)
SHAPE_REPRESENTATION_RELATIONSHIP()
);
#75=(
REPRESENTATION_RELATIONSHIP($,$,#11376,#11360)
REPRESENTATION_RELATIONSHIP_WITH_TRANSFORMATION(#37)
SHAPE_REPRESENTATION_RELATIONSHIP()
);
#76=(
REPRESENTATION_RELATIONSHIP($,$,#11377,#11360)
REPRESENTATION_RELATIONSHIP_WITH_TRANSFORMATION(#38)
SHAPE_REPRESENTATION_RELATIONSHIP()
);
#77=(
REPRESENTATION_RELATIONSHIP($,$,#11376,#11360)
REPRESENTATION_RELATIONSHIP_WITH_TRANSFORMATION(#39)
SHAPE_REPRESENTATION_RELATIONSHIP()
);
#78=(
REPRESENTATION_RELATIONSHIP($,$,#11377,#11360)
REPRESENTATION_RELATIONSHIP_WITH_TRANSFORMATION(#40)
SHAPE_REPRESENTATION_RELATIONSHIP()
);
#79=(
REPRESENTATION_RELATIONSHIP($,$,#11376,#11360)
REPRESENTATION_RELATIONSHIP_WITH_TRANSFORMATION(#41)
SHAPE_REPRESENTATION_RELATIONSHIP()
);
#80=(
REPRESENTATION_RELATIONSHIP($,$,#11376,#11360)
REPRESENTATION_RELATIONSHIP_WITH_TRANSFORMATION(#42)
SHAPE_REPRESENTATION_RELATIONSHIP()
);
#81=(
REPRESENTATION_RELATIONSHIP($,$,#11377,#11360)
REPRESENTATION_RELATIONSHIP_WITH_TRANSFORMATION(#43)
SHAPE_REPRESENTATION_RELATIONSHIP()
);
#82=(
REPRESENTATION_RELATIONSHIP($,$,#11377,#11360)
REPRESENTATION_RELATIONSHIP_WITH_TRANSFORMATION(#44)
SHAPE_REPRESENTATION_RELATIONSHIP()
);
#83=(
REPRESENTATION_RELATIONSHIP($,$,#11378,#11360)
REPRESENTATION_RELATIONSHIP_WITH_TRANSFORMATION(#45)
SHAPE_REPRESENTATION_RELATIONSHIP()
);
#84=(
REPRESENTATION_RELATIONSHIP($,$,#11380,#11379)
REPRESENTATION_RELATIONSHIP_WITH_TRANSFORMATION(#46)
SHAPE_REPRESENTATION_RELATIONSHIP()
);
#85=(
REPRESENTATION_RELATIONSHIP($,$,#11381,#11379)
REPRESENTATION_RELATIONSHIP_WITH_TRANSFORMATION(#47)
SHAPE_REPRESENTATION_RELATIONSHIP()
);
#86=(
REPRESENTATION_RELATIONSHIP($,$,#11382,#11379)
REPRESENTATION_RELATIONSHIP_WITH_TRANSFORMATION(#48)
SHAPE_REPRESENTATION_RELATIONSHIP()
);
#87=(
REPRESENTATION_RELATIONSHIP($,$,#11383,#11379)
REPRESENTATION_RELATIONSHIP_WITH_TRANSFORMATION(#49)
SHAPE_REPRESENTATION_RELATIONSHIP()
);
#88=(
REPRESENTATION_RELATIONSHIP($,$,#11384,#11379)
REPRESENTATION_RELATIONSHIP_WITH_TRANSFORMATION(#50)
SHAPE_REPRESENTATION_RELATIONSHIP()
);
#89=(
REPRESENTATION_RELATIONSHIP($,$,#11385,#11379)
REPRESENTATION_RELATIONSHIP_WITH_TRANSFORMATION(#51)
SHAPE_REPRESENTATION_RELATIONSHIP()
);
#90=(
REPRESENTATION_RELATIONSHIP($,$,#11387,#11386)
REPRESENTATION_RELATIONSHIP_WITH_TRANSFORMATION(#52)
SHAPE_REPRESENTATION_RELATIONSHIP()
);
#91=(
REPRESENTATION_RELATIONSHIP($,$,#11360,#11359)
REPRESENTATION_RELATIONSHIP_WITH_TRANSFORMATION(#53)
SHAPE_REPRESENTATION_RELATIONSHIP()
);
#92=(
REPRESENTATION_RELATIONSHIP($,$,#11379,#11359)
REPRESENTATION_RELATIONSHIP_WITH_TRANSFORMATION(#54)
SHAPE_REPRESENTATION_RELATIONSHIP()
);
#93=(
REPRESENTATION_RELATIONSHIP($,$,#11386,#11359)
REPRESENTATION_RELATIONSHIP_WITH_TRANSFORMATION(#55)
SHAPE_REPRESENTATION_RELATIONSHIP()
);
#94=CONTEXT_DEPENDENT_SHAPE_REPRESENTATION(#56,#11309);
#95=CONTEXT_DEPENDENT_SHAPE_REPRESENTATION(#57,#11310);
#96=CONTEXT_DEPENDENT_SHAPE_REPRESENTATION(#58,#11311);
#97=CONTEXT_DEPENDENT_SHAPE_REPRESENTATION(#59,#11312);
#98=CONTEXT_DEPENDENT_SHAPE_REPRESENTATION(#60,#11313);
#99=CONTEXT_DEPENDENT_SHAPE_REPRESENTATION(#61,#11317);
#100=CONTEXT_DEPENDENT_SHAPE_REPRESENTATION(#62,#11318);
#101=CONTEXT_DEPENDENT_SHAPE_REPRESENTATION(#63,#11319);
#102=CONTEXT_DEPENDENT_SHAPE_REPRESENTATION(#64,#11320);
#103=CONTEXT_DEPENDENT_SHAPE_REPRESENTATION(#65,#11321);
#104=CONTEXT_DEPENDENT_SHAPE_REPRESENTATION(#66,#11322);
#105=CONTEXT_DEPENDENT_SHAPE_REPRESENTATION(#67,#11323);
#106=CONTEXT_DEPENDENT_SHAPE_REPRESENTATION(#68,#11324);
#107=CONTEXT_DEPENDENT_SHAPE_REPRESENTATION(#69,#11325);
#108=CONTEXT_DEPENDENT_SHAPE_REPRESENTATION(#70,#11326);
#109=CONTEXT_DEPENDENT_SHAPE_REPRESENTATION(#71,#11327);
#110=CONTEXT_DEPENDENT_SHAPE_REPRESENTATION(#72,#11328);
#111=CONTEXT_DEPENDENT_SHAPE_REPRESENTATION(#73,#11329);
#112=CONTEXT_DEPENDENT_SHAPE_REPRESENTATION(#74,#11330);
#113=CONTEXT_DEPENDENT_SHAPE_REPRESENTATION(#75,#11331);
#114=CONTEXT_DEPENDENT_SHAPE_REPRESENTATION(#76,#11332);
#115=CONTEXT_DEPENDENT_SHAPE_REPRESENTATION(#77,#11333);
#116=CONTEXT_DEPENDENT_SHAPE_REPRESENTATION(#78,#11334);
#117=CONTEXT_DEPENDENT_SHAPE_REPRESENTATION(#79,#11335);
#118=CONTEXT_DEPENDENT_SHAPE_REPRESENTATION(#80,#11336);
#119=CONTEXT_DEPENDENT_SHAPE_REPRESENTATION(#81,#11337);
#120=CONTEXT_DEPENDENT_SHAPE_REPRESENTATION(#82,#11338);
#121=CONTEXT_DEPENDENT_SHAPE_REPRESENTATION(#83,#11339);
#122=CONTEXT_DEPENDENT_SHAPE_REPRESENTATION(#84,#11347);
#123=CONTEXT_DEPENDENT_SHAPE_REPRESENTATION(#85,#11348);
#124=CONTEXT_DEPENDENT_SHAPE_REPRESENTATION(#86,#11349);
#125=CONTEXT_DEPENDENT_SHAPE_REPRESENTATION(#87,#11350);
#126=CONTEXT_DEPENDENT_SHAPE_REPRESENTATION(#88,#11351);
#127=CONTEXT_DEPENDENT_SHAPE_REPRESENTATION(#89,#11352);
#128=CONTEXT_DEPENDENT_SHAPE_REPRESENTATION(#90,#11355);
#129=CONTEXT_DEPENDENT_SHAPE_REPRESENTATION(#91,#11356);
#130=CONTEXT_DEPENDENT_SHAPE_REPRESENTATION(#92,#11357);
#131=CONTEXT_DEPENDENT_SHAPE_REPRESENTATION(#93,#11358);
#132=NEXT_ASSEMBLY_USAGE_OCCURRENCE('Inner ring:1','Inner ring:1',
'Inner ring:1',#11400,#11401,'Inner ring:1');
#133=NEXT_ASSEMBLY_USAGE_OCCURRENCE('Outer ring:1','Outer ring:1',
'Outer ring:1',#11400,#11402,'Outer ring:1');
#134=NEXT_ASSEMBLY_USAGE_OCCURRENCE('Balls:1','Balls:1','Balls:1',#11400,
#11403,'Balls:1');
#135=NEXT_ASSEMBLY_USAGE_OCCURRENCE('Cage:1','Cage:1','Cage:1',#11400,#11404,
'Cage:1');
#136=NEXT_ASSEMBLY_USAGE_OCCURRENCE('Seals 2RS:1','Seals 2RS:1',
'Seals 2RS:1',#11400,#11405,'Seals 2RS:1');
#137=NEXT_ASSEMBLY_USAGE_OCCURRENCE('Ratchet demonstrator base:1',
'Ratchet demonstrator base:1','Ratchet demonstrator base:1',#11390,#11391,
'Ratchet demonstrator base:1');
#138=NEXT_ASSEMBLY_USAGE_OCCURRENCE('Pawl pivot pedestal:1',
'Pawl pivot pedestal:1','Pawl pivot pedestal:1',#11390,#11392,
'Pawl pivot pedestal:1');
#139=NEXT_ASSEMBLY_USAGE_OCCURRENCE('Pawl pivot pin:1',
'Pawl pivot pin:1','Pawl pivot pin:1',#11390,#11393,'Pawl pivot pin:1');
#140=NEXT_ASSEMBLY_USAGE_OCCURRENCE('Lower pawl spacer:1',
'Lower pawl spacer:1','Lower pawl spacer:1',#11390,#11394,
'Lower pawl spacer:1');
#141=NEXT_ASSEMBLY_USAGE_OCCURRENCE('Torsion spring guide:1',
'Torsion spring guide:1','Torsion spring guide:1',#11390,#11395,
'Torsion spring guide:1');
#142=NEXT_ASSEMBLY_USAGE_OCCURRENCE('Spring and pawl keeper:1',
'Spring and pawl keeper:1','Spring and pawl keeper:1',#11390,#11396,
'Spring and pawl keeper:1');
#143=NEXT_ASSEMBLY_USAGE_OCCURRENCE('Fixed spring anchor:1',
'Fixed spring anchor:1','Fixed spring anchor:1',#11390,#11397,
'Fixed spring anchor:1');
#144=NEXT_ASSEMBLY_USAGE_OCCURRENCE('Pivot pedestal:2',
'Pivot pedestal:2','Pivot pedestal:2',#11390,#11398,'Pivot pedestal:2');
#145=NEXT_ASSEMBLY_USAGE_OCCURRENCE('Pivot cap:2','Pivot cap:2',
'Pivot cap:2',#11390,#11399,'Pivot cap:2');
#146=NEXT_ASSEMBLY_USAGE_OCCURRENCE(
'Sealed Ball Bearing - 10 x 30 x 9 mm:2',
'Sealed Ball Bearing - 10 x 30 x 9 mm:2',
'Sealed Ball Bearing - 10 x 30 x 9 mm:2',#11390,#11400,
'Sealed Ball Bearing - 10 x 30 x 9 mm:2');
#147=NEXT_ASSEMBLY_USAGE_OCCURRENCE('M5x14 Cap Screw:2',
'M5x14 Cap Screw:2','M5x14 Cap Screw:2',#11390,#11406,
'M5x14 Cap Screw:2');
#148=NEXT_ASSEMBLY_USAGE_OCCURRENCE('M4x10 Cap Screw:2',
'M4x10 Cap Screw:2','M4x10 Cap Screw:2',#11390,#11407,
'M4x10 Cap Screw:2');
#149=NEXT_ASSEMBLY_USAGE_OCCURRENCE('M5x14 Cap Screw:3',
'M5x14 Cap Screw:3','M5x14 Cap Screw:3',#11390,#11406,
'M5x14 Cap Screw:3');
#150=NEXT_ASSEMBLY_USAGE_OCCURRENCE('M4x10 Cap Screw:3',
'M4x10 Cap Screw:3','M4x10 Cap Screw:3',#11390,#11407,
'M4x10 Cap Screw:3');
#151=NEXT_ASSEMBLY_USAGE_OCCURRENCE('M5x14 Cap Screw:4',
'M5x14 Cap Screw:4','M5x14 Cap Screw:4',#11390,#11406,
'M5x14 Cap Screw:4');
#152=NEXT_ASSEMBLY_USAGE_OCCURRENCE('M4x10 Cap Screw:4',
'M4x10 Cap Screw:4','M4x10 Cap Screw:4',#11390,#11407,
'M4x10 Cap Screw:4');
#153=NEXT_ASSEMBLY_USAGE_OCCURRENCE('M5x14 Cap Screw:5',
'M5x14 Cap Screw:5','M5x14 Cap Screw:5',#11390,#11406,
'M5x14 Cap Screw:5');
#154=NEXT_ASSEMBLY_USAGE_OCCURRENCE('M4x10 Cap Screw:5',
'M4x10 Cap Screw:5','M4x10 Cap Screw:5',#11390,#11407,
'M4x10 Cap Screw:5');
#155=NEXT_ASSEMBLY_USAGE_OCCURRENCE('M5x14 Cap Screw:6',
'M5x14 Cap Screw:6','M5x14 Cap Screw:6',#11390,#11406,
'M5x14 Cap Screw:6');
#156=NEXT_ASSEMBLY_USAGE_OCCURRENCE('M5x14 Cap Screw:7',
'M5x14 Cap Screw:7','M5x14 Cap Screw:7',#11390,#11406,
'M5x14 Cap Screw:7');
#157=NEXT_ASSEMBLY_USAGE_OCCURRENCE('M4x10 Cap Screw:6',
'M4x10 Cap Screw:6','M4x10 Cap Screw:6',#11390,#11407,
'M4x10 Cap Screw:6');
#158=NEXT_ASSEMBLY_USAGE_OCCURRENCE('M4x10 Cap Screw:7',
'M4x10 Cap Screw:7','M4x10 Cap Screw:7',#11390,#11407,
'M4x10 Cap Screw:7');
#159=NEXT_ASSEMBLY_USAGE_OCCURRENCE(
'Torsion Spring - 1.6 mm Wire, 12 mm Coil, 4.75 Turns:2',
'Torsion Spring - 1.6 mm Wire, 12 mm Coil, 4.75 Turns:2',
'Torsion Spring - 1.6 mm Wire, 12 mm Coil, 4.75 Turns:2',#11390,#11408,
'Torsion Spring - 1.6 mm Wire, 12 mm Coil, 4.75 Turns:2');
#160=NEXT_ASSEMBLY_USAGE_OCCURRENCE('Stepped ratchet spindle:1',
'Stepped ratchet spindle:1','Stepped ratchet spindle:1',#11409,#11410,
'Stepped ratchet spindle:1');
#161=NEXT_ASSEMBLY_USAGE_OCCURRENCE('Lower race sleeve:2',
'Lower race sleeve:2','Lower race sleeve:2',#11409,#11411,
'Lower race sleeve:2');
#162=NEXT_ASSEMBLY_USAGE_OCCURRENCE('Spindle collar:2',
'Spindle collar:2','Spindle collar:2',#11409,#11412,'Spindle collar:2');
#163=NEXT_ASSEMBLY_USAGE_OCCURRENCE('M4x4 collar screw:2',
'M4x4 collar screw:2','M4x4 collar screw:2',#11409,#11413,
'M4x4 collar screw:2');
#164=NEXT_ASSEMBLY_USAGE_OCCURRENCE('Ratchet wheel:2','Ratchet wheel:2',
'Ratchet wheel:2',#11409,#11414,'Ratchet wheel:2');
#165=NEXT_ASSEMBLY_USAGE_OCCURRENCE('Socket Set Screw - M5x8:2',
'Socket Set Screw - M5x8:2','Socket Set Screw - M5x8:2',#11409,#11415,
'Socket Set Screw - M5x8:2');
#166=NEXT_ASSEMBLY_USAGE_OCCURRENCE('Pawl with spring reaction tab:2',
'Pawl with spring reaction tab:2','Pawl with spring reaction tab:2',#11416,
#11417,'Pawl with spring reaction tab:2');
#167=NEXT_ASSEMBLY_USAGE_OCCURRENCE('Base bearings and spring anchor:1',
'Base bearings and spring anchor:1','Base bearings and spring anchor:1',
#11389,#11390,'Base bearings and spring anchor:1');
#168=NEXT_ASSEMBLY_USAGE_OCCURRENCE('Ratchet wheel and spindle:1',
'Ratchet wheel and spindle:1','Ratchet wheel and spindle:1',#11389,#11409,
'Ratchet wheel and spindle:1');
#169=NEXT_ASSEMBLY_USAGE_OCCURRENCE('Spring-biased pawl:1',
'Spring-biased pawl:1','Spring-biased pawl:1',#11389,#11416,
'Spring-biased pawl:1');
#170=SPHERICAL_SURFACE('',#5722,0.23815);
#171=SPHERICAL_SURFACE('',#5724,0.23815);
#172=SPHERICAL_SURFACE('',#5726,0.23815);
#173=SPHERICAL_SURFACE('',#5728,0.23815);
#174=SPHERICAL_SURFACE('',#5730,0.23815);
#175=SPHERICAL_SURFACE('',#5732,0.23815);
#176=SPHERICAL_SURFACE('',#5734,0.23815);
#177=SPHERICAL_SURFACE('',#5736,0.23815);
#178=SPHERICAL_SURFACE('',#5739,0.247676);
#179=SPHERICAL_SURFACE('',#5755,0.247676);
#180=SPHERICAL_SURFACE('',#5760,0.247676);
#181=SPHERICAL_SURFACE('',#5765,0.247676);
#182=SPHERICAL_SURFACE('',#5770,0.247676);
#183=SPHERICAL_SURFACE('',#5775,0.247676);
#184=SPHERICAL_SURFACE('',#5780,0.247676);
#185=SPHERICAL_SURFACE('',#5788,0.247676);
#186=CONICAL_SURFACE('',#5693,0.53,0.785398163397448);
#187=CONICAL_SURFACE('',#5700,0.53,0.785398163397448);
#188=CONICAL_SURFACE('',#5713,1.47,0.785398163397449);
#189=CONICAL_SURFACE('',#5717,1.47,0.785398163397449);
#190=CONICAL_SURFACE('',#5827,0.4,0.785398163397448);
#191=CONICAL_SURFACE('',#5831,0.41,0.785398163397448);
#192=CONICAL_SURFACE('',#5835,0.26,0.463647609000806);
#193=CONICAL_SURFACE('',#5851,0.325,0.785398163397448);
#194=CONICAL_SURFACE('',#5855,0.335,0.785398163397448);
#195=CONICAL_SURFACE('',#5859,0.21,0.463647609000806);
#196=CONICAL_SURFACE('',#5944,0.185,0.785398163397449);
#197=CONICAL_SURFACE('',#6021,0.235,0.785398163397448);
#198=CONICAL_SURFACE('',#6025,0.2125,0.785398163397448);
#199=TOROIDAL_SURFACE('',#5682,1.,0.247676);
#200=TOROIDAL_SURFACE('',#5702,1.,0.247676);
#201=B_SPLINE_CURVE_WITH_KNOTS('',3,(#7931,#7932,#7933,#7934,#7935,#7936,
#7937,#7938,#7939,#7940),.UNSPECIFIED.,.F.,.F.,(4,2,2,2,4),(0.,0.0945941824764479,
0.189188364952896,0.283770357603024,0.378352350253152),.UNSPECIFIED.);
#202=B_SPLINE_CURVE_WITH_KNOTS('',3,(#7941,#7942,#7943,#7944,#7945,#7946,
#7947,#7948,#7949,#7950,#7951,#7952,#7953,#7954,#7955,#7956,#7957,#7958,
#7959,#7960,#7961,#7962,#7963,#7964,#7965,#7966),.UNSPECIFIED.,.F.,.F.,
(4,2,2,2,2,2,2,2,2,2,2,2,4),(0.378352350253152,0.47293434290328,0.567516335553408,
0.662110518029855,0.756704700506303,0.851298882982751,0.945893065459199,
1.04047505810933,1.13505705075946,1.22963904340958,1.32422103605971,1.41881521853616,
1.51340940101261),.UNSPECIFIED.);
#203=B_SPLINE_CURVE_WITH_KNOTS('',3,(#7970,#7971,#7972,#7973,#7974,#7975,
#7976,#7977,#7978,#7979,#7980,#7981,#7982,#7983,#7984,#7985,#7986,#7987,
#7988,#7989,#7990,#7991,#7992,#7993,#7994,#7995),.UNSPECIFIED.,.F.,.F.,
(4,2,2,2,2,2,2,2,2,2,2,2,4),(0.,0.0942186410044058,0.188437282008812,0.282655768798837,
0.376874255588861,0.471092742378886,0.565311229168911,0.659529870173317,
0.753748511177723,0.847967152182129,0.942185793186535,1.03640427997656,
1.13062276676658),.UNSPECIFIED.);
#204=B_SPLINE_CURVE_WITH_KNOTS('',3,(#7996,#7997,#7998,#7999,#8000,#8001,
#8002,#8003,#8004,#8005),.UNSPECIFIED.,.F.,.F.,(4,2,2,2,4),(1.13062276676658,
1.22484125355661,1.31905974034663,1.41327838135104,1.50749702235545),
 .UNSPECIFIED.);
#205=B_SPLINE_CURVE_WITH_KNOTS('',3,(#8316,#8317,#8318,#8319,#8320,#8321,
#8322,#8323,#8324,#8325,#8326,#8327,#8328,#8329,#8330,#8331,#8332,#8333,
#8334,#8335,#8336,#8337),.UNSPECIFIED.,.F.,.F.,(4,2,2,2,2,2,2,2,2,2,4),
(0.0473477652366656,0.126350602536658,0.189525903804987,0.252701205073317,
0.313298422430275,0.373895639787233,0.434492857144191,0.495090074501149,
0.558265375769478,0.621440677037807,0.7004435143378),.UNSPECIFIED.);
#206=B_SPLINE_CURVE_WITH_KNOTS('',3,(#8341,#8342,#8343,#8344,#8345,#8346,
#8347,#8348,#8349,#8350,#8351,#8352,#8353,#8354,#8355,#8356,#8357,#8358,
#8359,#8360,#8361,#8362),.UNSPECIFIED.,.F.,.F.,(4,2,2,2,2,2,2,2,2,2,4),
(0.0464897534940957,0.0852567806515119,0.170513561303024,0.246687263103517,
0.308657850341199,0.370628437578881,0.432599024816563,0.494569612054245,
0.570743313854739,0.656000094506251,0.694767121663666),.UNSPECIFIED.);
#207=B_SPLINE_CURVE_WITH_KNOTS('',3,(#8368,#8369,#8370,#8371,#8372,#8373,
#8374,#8375,#8376,#8377,#8378,#8379,#8380,#8381,#8382,#8383,#8384,#8385,
#8386,#8387,#8388,#8389),.UNSPECIFIED.,.F.,.F.,(4,2,2,2,2,2,2,2,2,2,4),
(0.0464897534940957,0.0852567806515118,0.170513561303024,0.246687263103517,
0.308657850341199,0.370628437578881,0.432599024816563,0.494569612054245,
0.570743313854738,0.65600009450625,0.694767121663666),.UNSPECIFIED.);
#208=B_SPLINE_CURVE_WITH_KNOTS('',3,(#8393,#8394,#8395,#8396,#8397,#8398,
#8399,#8400,#8401,#8402,#8403,#8404,#8405,#8406,#8407,#8408,#8409,#8410,
#8411,#8412,#8413,#8414),.UNSPECIFIED.,.F.,.F.,(4,2,2,2,2,2,2,2,2,2,4),
(0.0464897534940957,0.0852567806515119,0.170513561303024,0.246687263103517,
0.308657850341199,0.370628437578881,0.432599024816563,0.494569612054245,
0.570743313854739,0.656000094506251,0.694767121663666),.UNSPECIFIED.);
#209=B_SPLINE_CURVE_WITH_KNOTS('',3,(#8418,#8419,#8420,#8421,#8422,#8423,
#8424,#8425,#8426,#8427,#8428,#8429),.UNSPECIFIED.,.F.,.F.,(4,2,2,2,2,4),
(0.0464897534940957,0.0852567806515119,0.170513561303024,0.246687263103517,
0.308657850341199,0.370628437578881),.UNSPECIFIED.);
#210=B_SPLINE_CURVE_WITH_KNOTS('',3,(#8434,#8435,#8436,#8437,#8438,#8439,
#8440,#8441,#8442,#8443,#8444,#8445),.UNSPECIFIED.,.F.,.F.,(4,2,2,2,2,4),
(0.370628437578881,0.432599024816563,0.494569612054245,0.570743313854738,
0.65600009450625,0.694767121663666),.UNSPECIFIED.);
#211=B_SPLINE_CURVE_WITH_KNOTS('',3,(#8449,#8450,#8451,#8452,#8453,#8454,
#8455,#8456,#8457,#8458,#8459,#8460,#8461,#8462,#8463,#8464,#8465,#8466,
#8467,#8468,#8469,#8470),.UNSPECIFIED.,.F.,.F.,(4,2,2,2,2,2,2,2,2,2,4),
(0.0464897534940957,0.0852567806515121,0.170513561303024,0.246687263103518,
0.308657850341199,0.370628437578881,0.432599024816563,0.494569612054245,
0.570743313854738,0.65600009450625,0.694767121663666),.UNSPECIFIED.);
#212=B_SPLINE_CURVE_WITH_KNOTS('',3,(#8474,#8475,#8476,#8477,#8478,#8479,
#8480,#8481,#8482,#8483,#8484,#8485,#8486,#8487,#8488,#8489,#8490,#8491,
#8492,#8493,#8494,#8495),.UNSPECIFIED.,.F.,.F.,(4,2,2,2,2,2,2,2,2,2,4),
(0.0464897534940957,0.0852567806515119,0.170513561303024,0.246687263103517,
0.308657850341199,0.370628437578881,0.432599024816563,0.494569612054245,
0.570743313854738,0.65600009450625,0.694767121663667),.UNSPECIFIED.);
#213=B_SPLINE_CURVE_WITH_KNOTS('',3,(#8499,#8500,#8501,#8502,#8503,#8504,
#8505,#8506,#8507,#8508,#8509,#8510,#8511,#8512,#8513,#8514,#8515,#8516,
#8517,#8518,#8519,#8520),.UNSPECIFIED.,.F.,.F.,(4,2,2,2,2,2,2,2,2,2,4),
(0.0464897534940957,0.0852567806515119,0.170513561303024,0.246687263103517,
0.308657850341199,0.370628437578881,0.432599024816563,0.494569612054245,
0.570743313854738,0.65600009450625,0.694767121663666),.UNSPECIFIED.);
#214=B_SPLINE_CURVE_WITH_KNOTS('',3,(#8524,#8525,#8526,#8527,#8528,#8529,
#8530,#8531,#8532,#8533,#8534,#8535,#8536,#8537,#8538,#8539,#8540,#8541,
#8542,#8543,#8544,#8545),.UNSPECIFIED.,.F.,.F.,(4,2,2,2,2,2,2,2,2,2,4),
(0.0464897534940957,0.0852567806515119,0.170513561303024,0.246687263103517,
0.308657850341199,0.370628437578881,0.432599024816563,0.494569612054245,
0.570743313854739,0.656000094506251,0.694767121663667),.UNSPECIFIED.);
#215=B_SPLINE_CURVE_WITH_KNOTS('',3,(#8553,#8554,#8555,#8556,#8557,#8558,
#8559,#8560,#8561,#8562,#8563,#8564,#8565,#8566,#8567,#8568,#8569,#8570,
#8571,#8572,#8573,#8574),.UNSPECIFIED.,.F.,.F.,(4,2,2,2,2,2,2,2,2,2,4),
(0.0473477652366656,0.126350602536658,0.189525903804987,0.252701205073316,
0.313298422430274,0.373895639787232,0.434492857144191,0.495090074501149,
0.558265375769478,0.621440677037807,0.7004435143378),.UNSPECIFIED.);
#216=B_SPLINE_CURVE_WITH_KNOTS('',3,(#8582,#8583,#8584,#8585,#8586,#8587,
#8588,#8589,#8590,#8591,#8592,#8593,#8594,#8595,#8596,#8597,#8598,#8599,
#8600,#8601,#8602,#8603),.UNSPECIFIED.,.F.,.F.,(4,2,2,2,2,2,2,2,2,2,4),
(0.0473477652366656,0.126350602536658,0.189525903804987,0.252701205073317,
0.313298422430275,0.373895639787233,0.434492857144191,0.495090074501149,
0.558265375769478,0.621440677037807,0.7004435143378),.UNSPECIFIED.);
#217=B_SPLINE_CURVE_WITH_KNOTS('',3,(#8612,#8613,#8614,#8615,#8616,#8617,
#8618,#8619,#8620,#8621,#8622,#8623),.UNSPECIFIED.,.F.,.F.,(4,2,2,2,2,4),
(0.0473477652366656,0.126350602536658,0.189525903804987,0.252701205073316,
0.313298422430275,0.373895639787233),.UNSPECIFIED.);
#218=B_SPLINE_CURVE_WITH_KNOTS('',3,(#8625,#8626,#8627,#8628,#8629,#8630,
#8631,#8632,#8633,#8634,#8635,#8636),.UNSPECIFIED.,.F.,.F.,(4,2,2,2,2,4),
(0.373895639787233,0.434492857144191,0.495090074501149,0.558265375769478,
0.621440677037807,0.7004435143378),.UNSPECIFIED.);
#219=B_SPLINE_CURVE_WITH_KNOTS('',3,(#8643,#8644,#8645,#8646,#8647,#8648,
#8649,#8650,#8651,#8652,#8653,#8654,#8655,#8656,#8657,#8658,#8659,#8660,
#8661,#8662,#8663,#8664),.UNSPECIFIED.,.F.,.F.,(4,2,2,2,2,2,2,2,2,2,4),
(0.0473477652366656,0.126350602536658,0.189525903804987,0.252701205073316,
0.313298422430275,0.373895639787233,0.434492857144191,0.495090074501149,
0.558265375769478,0.621440677037807,0.7004435143378),.UNSPECIFIED.);
#220=B_SPLINE_CURVE_WITH_KNOTS('',3,(#8672,#8673,#8674,#8675,#8676,#8677,
#8678,#8679,#8680,#8681,#8682,#8683,#8684,#8685,#8686,#8687,#8688,#8689,
#8690,#8691,#8692,#8693),.UNSPECIFIED.,.F.,.F.,(4,2,2,2,2,2,2,2,2,2,4),
(0.0473477652366656,0.126350602536658,0.189525903804987,0.252701205073317,
0.313298422430275,0.373895639787233,0.434492857144191,0.495090074501149,
0.558265375769478,0.621440677037807,0.7004435143378),.UNSPECIFIED.);
#221=B_SPLINE_CURVE_WITH_KNOTS('',3,(#8701,#8702,#8703,#8704,#8705,#8706,
#8707,#8708,#8709,#8710,#8711,#8712,#8713,#8714,#8715,#8716,#8717,#8718,
#8719,#8720,#8721,#8722),.UNSPECIFIED.,.F.,.F.,(4,2,2,2,2,2,2,2,2,2,4),
(0.0473477652366656,0.126350602536658,0.189525903804987,0.252701205073316,
0.313298422430275,0.373895639787233,0.434492857144191,0.495090074501149,
0.558265375769478,0.621440677037807,0.7004435143378),.UNSPECIFIED.);
#222=B_SPLINE_CURVE_WITH_KNOTS('',3,(#8731,#8732,#8733,#8734,#8735,#8736,
#8737,#8738,#8739,#8740,#8741,#8742,#8743,#8744,#8745,#8746,#8747,#8748,
#8749,#8750,#8751,#8752),.UNSPECIFIED.,.F.,.F.,(4,2,2,2,2,2,2,2,2,2,4),
(0.0473477652366656,0.126350602536658,0.189525903804987,0.252701205073317,
0.313298422430275,0.373895639787233,0.434492857144191,0.495090074501149,
0.558265375769478,0.621440677037807,0.7004435143378),.UNSPECIFIED.);
#223=B_SPLINE_CURVE_WITH_KNOTS('',3,(#9532,#9533,#9534,#9535,#9536,#9537,
#9538,#9539,#9540,#9541,#9542,#9543,#9544,#9545,#9546,#9547,#9548,#9549,
#9550,#9551,#9552,#9553,#9554,#9555,#9556,#9557,#9558,#9559,#9560,#9561,
#9562,#9563,#9564,#9565,#9566,#9567,#9568,#9569,#9570,#9571,#9572,#9573,
#9574,#9575,#9576,#9577,#9578,#9579,#9580,#9581,#9582,#9583,#9584,#9585,
#9586,#9587,#9588,#9589,#9590,#9591,#9592,#9593,#9594,#9595,#9596,#9597,
#9598),.UNSPECIFIED.,.F.,.F.,(4,1,1,1,1,1,1,1,1,1,1,1,1,1,1,1,1,1,1,1,1,
1,1,1,1,1,1,1,1,1,1,1,1,1,1,1,1,1,1,1,1,1,1,1,1,1,1,1,1,1,1,1,1,1,1,1,1,
1,1,1,1,1,1,1,4),(-1.,-0.982142857142857,-0.964285714285714,-0.955357142857143,
-0.946428571428571,-0.9375,-0.928571428571429,-0.919642857142857,-0.915178571428571,
-0.910714285714286,-0.901785714285714,-0.892857142857143,-0.875,-0.866071428571429,
-0.861607142857143,-0.857142857142857,-0.833333333333333,-0.809523809523809,
-0.785714285714286,-0.761904761904762,-0.746031746031746,-0.73015873015873,
-0.714285714285714,-0.698412698412698,-0.682539682539682,-0.666666666666667,
-0.642857142857143,-0.619047619047619,-0.595238095238095,-0.571428571428571,
-0.547619047619048,-0.523809523809524,-0.507936507936508,-0.492063492063492,
-0.476190476190476,-0.452380952380952,-0.428571428571429,-0.410714285714286,
-0.392857142857143,-0.369047619047619,-0.357142857142857,-0.339285714285714,
-0.321428571428571,-0.303571428571429,-0.285714285714286,-0.267857142857143,
-0.25,-0.232142857142857,-0.214285714285714,-0.19047619047619,-0.166666666666667,
-0.142857142857143,-0.125,-0.107142857142857,-0.0982142857142857,-0.0892857142857143,
-0.0848214285714286,-0.0803571428571428,-0.0714285714285714,-0.0625,-0.0535714285714286,
-0.0446428571428571,-0.0357142857142857,-0.0178571428571429,0.),
 .UNSPECIFIED.);
#224=B_SPLINE_CURVE_WITH_KNOTS('',3,(#9602,#9603,#9604,#9605,#9606,#9607,
#9608,#9609,#9610,#9611,#9612,#9613,#9614,#9615,#9616,#9617,#9618,#9619,
#9620,#9621,#9622,#9623,#9624,#9625,#9626,#9627,#9628,#9629,#9630,#9631,
#9632,#9633,#9634,#9635,#9636,#9637,#9638,#9639,#9640,#9641,#9642,#9643,
#9644,#9645,#9646,#9647,#9648,#9649,#9650,#9651,#9652,#9653,#9654,#9655,
#9656,#9657,#9658,#9659,#9660,#9661,#9662,#9663,#9664,#9665,#9666,#9667,
#9668),.UNSPECIFIED.,.F.,.F.,(4,1,1,1,1,1,1,1,1,1,1,1,1,1,1,1,1,1,1,1,1,
1,1,1,1,1,1,1,1,1,1,1,1,1,1,1,1,1,1,1,1,1,1,1,1,1,1,1,1,1,1,1,1,1,1,1,1,
1,1,1,1,1,1,1,4),(-1.,-0.982142857142857,-0.964285714285714,-0.955357142857143,
-0.946428571428571,-0.9375,-0.928571428571429,-0.919642857142857,-0.915178571428571,
-0.910714285714286,-0.901785714285714,-0.892857142857143,-0.875,-0.866071428571429,
-0.861607142857143,-0.857142857142857,-0.833333333333333,-0.809523809523809,
-0.785714285714286,-0.761904761904762,-0.746031746031746,-0.73015873015873,
-0.714285714285714,-0.698412698412698,-0.682539682539682,-0.666666666666667,
-0.642857142857143,-0.619047619047619,-0.595238095238095,-0.571428571428571,
-0.547619047619048,-0.523809523809524,-0.507936507936508,-0.492063492063492,
-0.476190476190476,-0.452380952380952,-0.428571428571429,-0.410714285714286,
-0.392857142857143,-0.369047619047619,-0.357142857142857,-0.339285714285714,
-0.321428571428571,-0.303571428571429,-0.285714285714286,-0.267857142857143,
-0.25,-0.232142857142857,-0.214285714285714,-0.19047619047619,-0.166666666666667,
-0.142857142857143,-0.125,-0.107142857142857,-0.0982142857142857,-0.0892857142857143,
-0.0848214285714286,-0.0803571428571428,-0.0714285714285714,-0.0625,-0.0535714285714286,
-0.0446428571428571,-0.0357142857142857,-0.0178571428571429,0.),
 .UNSPECIFIED.);
#225=B_SPLINE_CURVE_WITH_KNOTS('',3,(#9957,#9958,#9959,#9960,#9961,#9962,
#9963,#9964,#9965,#9966,#9967,#9968,#9969,#9970,#9971,#9972,#9973,#9974,
#9975,#9976,#9977,#9978,#9979,#9980,#9981,#9982,#9983,#9984,#9985,#9986,
#9987,#9988,#9989,#9990,#9991,#9992,#9993,#9994,#9995,#9996,#9997,#9998,
#9999,#10000,#10001,#10002,#10003,#10004,#10005,#10006,#10007,#10008,#10009,
#10010,#10011,#10012,#10013,#10014,#10015,#10016,#10017,#10018,#10019,#10020,
#10021,#10022,#10023,#10024,#10025,#10026,#10027),.UNSPECIFIED.,.F.,.F.,
(4,1,1,1,1,1,1,1,1,1,1,1,1,1,1,1,1,1,1,1,1,1,1,1,1,1,1,1,1,1,1,1,1,1,1,
1,1,1,1,1,1,1,1,1,1,1,1,1,1,1,1,1,1,1,1,1,1,1,1,1,1,1,1,1,1,1,1,1,4),(0.,
0.0178571428571429,0.0357142857142857,0.0446428571428571,0.0535714285714286,
0.0625,0.0714285714285714,0.0803571428571428,0.0892857142857143,0.0982142857142857,
0.107142857142857,0.125,0.142857142857143,0.166666666666667,0.19047619047619,
0.196428571428571,0.214285714285714,0.232142857142857,0.25,0.267857142857143,
0.285714285714286,0.303571428571429,0.321428571428571,0.339285714285714,
0.357142857142857,0.369047619047619,0.392857142857143,0.410714285714286,
0.419642857142857,0.428571428571429,0.452380952380952,0.476190476190476,
0.492063492063492,0.5,0.507936507936508,0.523809523809524,0.547619047619048,
0.571428571428571,0.595238095238095,0.619047619047619,0.642857142857143,
0.666666666666667,0.682539682539682,0.698412698412698,0.714285714285714,
0.722222222222222,0.73015873015873,0.746031746031746,0.761904761904762,
0.773809523809524,0.785714285714286,0.809523809523809,0.833333333333333,
0.857142857142857,0.859375,0.861607142857143,0.866071428571429,0.875,0.892857142857143,
0.901785714285714,0.910714285714286,0.919642857142857,0.928571428571429,
0.9375,0.946428571428571,0.955357142857143,0.964285714285714,0.982142857142857,
1.),.UNSPECIFIED.);
#226=B_SPLINE_CURVE_WITH_KNOTS('',3,(#10535,#10536,#10537,#10538,#10539,
#10540,#10541,#10542,#10543,#10544,#10545,#10546,#10547,#10548),
 .UNSPECIFIED.,.F.,.F.,(4,2,2,2,2,2,4),(0.618551524396293,0.626563103102765,
0.689203386094988,0.751843669087211,0.814483952079434,0.877124235071657,
0.88513581377813),.UNSPECIFIED.);
#227=B_SPLINE_CURVE_WITH_KNOTS('',3,(#10552,#10553,#10554,#10555,#10556,
#10557,#10558,#10559),.UNSPECIFIED.,.F.,.F.,(4,2,2,4),(0.250614556362404,
0.313254839354627,0.37589512234685,0.383906701053323),.UNSPECIFIED.);
#228=B_SPLINE_CURVE_WITH_KNOTS('',3,(#10563,#10564,#10565,#10566,#10567,
#10568,#10569,#10570,#10571,#10572,#10573,#10574,#10575,#10576,#10577,#10578,
#10579,#10580,#10581,#10582,#10583,#10584,#10585,#10586,#10587,#10588),
 .UNSPECIFIED.,.F.,.F.,(4,2,2,2,2,2,2,2,2,2,2,2,4),(0.,0.0623062782223143,
0.124612556444629,0.186916384615149,0.249220212785669,0.31152404095619,
0.37382786912671,0.436134147349024,0.498440425571339,0.560746703793653,
0.623052982015967,0.685356810186488,0.747660638357008),.UNSPECIFIED.);
#229=B_SPLINE_CURVE_WITH_KNOTS('',3,(#10589,#10590,#10591,#10592,#10593,
#10594,#10595,#10596,#10597,#10598),.UNSPECIFIED.,.F.,.F.,(4,2,2,2,4),(0.747660638357008,
0.809964466527528,0.872268294698049,0.934574572920363,0.996880851142677),
 .UNSPECIFIED.);
#230=B_SPLINE_CURVE_WITH_KNOTS('',3,(#10599,#10600,#10601,#10602,#10603,
#10604,#10605,#10606),.UNSPECIFIED.,.F.,.F.,(4,2,2,4),(0.117322411671485,
0.125333990377958,0.187974273370181,0.250614556362404),.UNSPECIFIED.);
#231=B_SPLINE_CURVE_WITH_KNOTS('',3,(#10681,#10682,#10683,#10684,#10685,
#10686,#10687,#10688,#10689,#10690,#10691,#10692,#10693,#10694),
 .UNSPECIFIED.,.F.,.F.,(4,2,2,2,2,2,4),(0.75600573798702,0.793568827564647,
0.872922520054201,0.952276212543756,1.03162990503331,1.11098359752287,1.14854668710049),
 .UNSPECIFIED.);
#232=B_SPLINE_CURVE_WITH_KNOTS('',3,(#10700,#10701,#10702,#10703,#10704,
#10705,#10706,#10707,#10708,#10709,#10710,#10711,#10712,#10713,#10714,#10715,
#10716,#10717),.UNSPECIFIED.,.F.,.F.,(4,2,2,2,2,2,2,2,4),(0.,0.0792028026112439,
0.158405605222488,0.237607602356377,0.316809599490267,0.396011596624156,
0.475213593758045,0.554416396369289,0.633619198980533),.UNSPECIFIED.);
#233=B_SPLINE_CURVE_WITH_KNOTS('',3,(#10718,#10719,#10720,#10721,#10722,
#10723,#10724,#10725,#10726,#10727,#10728,#10729,#10730,#10731,#10732,#10733,
#10734,#10735),.UNSPECIFIED.,.F.,.F.,(4,2,2,2,2,2,2,2,4),(0.633619198980533,
0.712822001591777,0.792024804203021,0.87122680133691,0.950428798470799,
1.02963079560469,1.10883279273858,1.18803559534982,1.26723839796107),
 .UNSPECIFIED.);
#234=B_SPLINE_CURVE_WITH_KNOTS('',3,(#10738,#10739,#10740,#10741,#10742,
#10743,#10744,#10745,#10746,#10747,#10748,#10749,#10750,#10751),
 .UNSPECIFIED.,.F.,.F.,(4,2,2,2,2,2,4),(0.121154929624516,0.158718019202143,
0.238071711691697,0.317425404181252,0.396779096670807,0.476132789160362,
0.513695878737989),.UNSPECIFIED.);
#235=SHAPE_REPRESENTATION_RELATIONSHIP('SRR','None',#11361,#259);
#236=SHAPE_REPRESENTATION_RELATIONSHIP('SRR','None',#11362,#260);
#237=SHAPE_REPRESENTATION_RELATIONSHIP('SRR','None',#11363,#261);
#238=SHAPE_REPRESENTATION_RELATIONSHIP('SRR','None',#11364,#262);
#239=SHAPE_REPRESENTATION_RELATIONSHIP('SRR','None',#11365,#263);
#240=SHAPE_REPRESENTATION_RELATIONSHIP('SRR','None',#11366,#264);
#241=SHAPE_REPRESENTATION_RELATIONSHIP('SRR','None',#11367,#265);
#242=SHAPE_REPRESENTATION_RELATIONSHIP('SRR','None',#11368,#266);
#243=SHAPE_REPRESENTATION_RELATIONSHIP('SRR','None',#11369,#267);
#244=SHAPE_REPRESENTATION_RELATIONSHIP('SRR','None',#11371,#268);
#245=SHAPE_REPRESENTATION_RELATIONSHIP('SRR','None',#11372,#269);
#246=SHAPE_REPRESENTATION_RELATIONSHIP('SRR','None',#11373,#270);
#247=SHAPE_REPRESENTATION_RELATIONSHIP('SRR','None',#11374,#271);
#248=SHAPE_REPRESENTATION_RELATIONSHIP('SRR','None',#11375,#272);
#249=SHAPE_REPRESENTATION_RELATIONSHIP('SRR','None',#11376,#273);
#250=SHAPE_REPRESENTATION_RELATIONSHIP('SRR','None',#11377,#274);
#251=SHAPE_REPRESENTATION_RELATIONSHIP('SRR','None',#11378,#275);
#252=SHAPE_REPRESENTATION_RELATIONSHIP('SRR','None',#11380,#276);
#253=SHAPE_REPRESENTATION_RELATIONSHIP('SRR','None',#11381,#277);
#254=SHAPE_REPRESENTATION_RELATIONSHIP('SRR','None',#11382,#278);
#255=SHAPE_REPRESENTATION_RELATIONSHIP('SRR','None',#11383,#279);
#256=SHAPE_REPRESENTATION_RELATIONSHIP('SRR','None',#11384,#280);
#257=SHAPE_REPRESENTATION_RELATIONSHIP('SRR','None',#11385,#281);
#258=SHAPE_REPRESENTATION_RELATIONSHIP('SRR','None',#11387,#282);
#259=ADVANCED_BREP_SHAPE_REPRESENTATION('',(#315),#11231);
#260=ADVANCED_BREP_SHAPE_REPRESENTATION('',(#316),#11232);
#261=ADVANCED_BREP_SHAPE_REPRESENTATION('',(#317),#11233);
#262=ADVANCED_BREP_SHAPE_REPRESENTATION('',(#318),#11234);
#263=ADVANCED_BREP_SHAPE_REPRESENTATION('',(#319),#11235);
#264=ADVANCED_BREP_SHAPE_REPRESENTATION('',(#320),#11236);
#265=ADVANCED_BREP_SHAPE_REPRESENTATION('',(#321),#11237);
#266=ADVANCED_BREP_SHAPE_REPRESENTATION('',(#322),#11238);
#267=ADVANCED_BREP_SHAPE_REPRESENTATION('',(#323),#11239);
#268=ADVANCED_BREP_SHAPE_REPRESENTATION('',(#324),#11241);
#269=ADVANCED_BREP_SHAPE_REPRESENTATION('',(#325),#11242);
#270=ADVANCED_BREP_SHAPE_REPRESENTATION('',(#326,#327,#328,#329,#330,#331,
#332,#333),#11243);
#271=ADVANCED_BREP_SHAPE_REPRESENTATION('',(#334),#11244);
#272=ADVANCED_BREP_SHAPE_REPRESENTATION('',(#335,#336),#11245);
#273=ADVANCED_BREP_SHAPE_REPRESENTATION('',(#16),#11246);
#274=ADVANCED_BREP_SHAPE_REPRESENTATION('',(#17),#11247);
#275=ADVANCED_BREP_SHAPE_REPRESENTATION('',(#337),#11248);
#276=ADVANCED_BREP_SHAPE_REPRESENTATION('',(#338),#11250);
#277=ADVANCED_BREP_SHAPE_REPRESENTATION('',(#339),#11251);
#278=ADVANCED_BREP_SHAPE_REPRESENTATION('',(#340),#11252);
#279=ADVANCED_BREP_SHAPE_REPRESENTATION('',(#341),#11253);
#280=ADVANCED_BREP_SHAPE_REPRESENTATION('',(#342),#11254);
#281=ADVANCED_BREP_SHAPE_REPRESENTATION('',(#343),#11255);
#282=ADVANCED_BREP_SHAPE_REPRESENTATION('',(#344),#11257);
#283=STYLED_ITEM('',(#11563),#315);
#284=STYLED_ITEM('',(#11577),#316);
#285=STYLED_ITEM('',(#11584),#317);
#286=STYLED_ITEM('',(#11598),#318);
#287=STYLED_ITEM('',(#11584),#319);
#288=STYLED_ITEM('',(#11584),#320);
#289=STYLED_ITEM('',(#11584),#321);
#290=STYLED_ITEM('',(#11598),#322);
#291=STYLED_ITEM('',(#11570),#323);
#292=STYLED_ITEM('',(#11584),#324);
#293=STYLED_ITEM('',(#11584),#325);
#294=STYLED_ITEM('',(#11584),#326);
#295=STYLED_ITEM('',(#11584),#327);
#296=STYLED_ITEM('',(#11584),#328);
#297=STYLED_ITEM('',(#11584),#329);
#298=STYLED_ITEM('',(#11584),#330);
#299=STYLED_ITEM('',(#11584),#331);
#300=STYLED_ITEM('',(#11584),#332);
#301=STYLED_ITEM('',(#11584),#333);
#302=STYLED_ITEM('',(#11584),#334);
#303=STYLED_ITEM('',(#11584),#335);
#304=STYLED_ITEM('',(#11584),#336);
#305=STYLED_ITEM('',(#11591),#16);
#306=STYLED_ITEM('',(#11591),#17);
#307=STYLED_ITEM('',(#11584),#337);
#308=STYLED_ITEM('',(#11577),#338);
#309=STYLED_ITEM('',(#11570),#339);
#310=STYLED_ITEM('',(#11577),#340);
#311=STYLED_ITEM('',(#11591),#341);
#312=STYLED_ITEM('',(#11577),#342);
#313=STYLED_ITEM('',(#11591),#343);
#314=STYLED_ITEM('',(#11584),#344);
#315=MANIFOLD_SOLID_BREP('Body1',#5154);
#316=MANIFOLD_SOLID_BREP('Body1',#5155);
#317=MANIFOLD_SOLID_BREP('Body1',#5156);
#318=MANIFOLD_SOLID_BREP('Body1',#5157);
#319=MANIFOLD_SOLID_BREP('Body1',#5158);
#320=MANIFOLD_SOLID_BREP('Body1',#5159);
#321=MANIFOLD_SOLID_BREP('Body1',#5160);
#322=MANIFOLD_SOLID_BREP('Body1',#5161);
#323=MANIFOLD_SOLID_BREP('Body1',#5162);
#324=MANIFOLD_SOLID_BREP('Body1',#5163);
#325=MANIFOLD_SOLID_BREP('Body1',#5164);
#326=MANIFOLD_SOLID_BREP('Body1',#5165);
#327=MANIFOLD_SOLID_BREP('Body2',#5166);
#328=MANIFOLD_SOLID_BREP('Body3',#5167);
#329=MANIFOLD_SOLID_BREP('Body4',#5168);
#330=MANIFOLD_SOLID_BREP('Body5',#5169);
#331=MANIFOLD_SOLID_BREP('Body6',#5170);
#332=MANIFOLD_SOLID_BREP('Body7',#5171);
#333=MANIFOLD_SOLID_BREP('Body8',#5172);
#334=MANIFOLD_SOLID_BREP('Continuous crown cage',#5173);
#335=MANIFOLD_SOLID_BREP('Body1',#5174);
#336=MANIFOLD_SOLID_BREP('Body2',#5175);
#337=MANIFOLD_SOLID_BREP('Body1',#5180);
#338=MANIFOLD_SOLID_BREP('Body1',#5181);
#339=MANIFOLD_SOLID_BREP('Body1',#5182);
#340=MANIFOLD_SOLID_BREP('Body1',#5183);
#341=MANIFOLD_SOLID_BREP('Body1',#5184);
#342=MANIFOLD_SOLID_BREP('Body1',#5185);
#343=MANIFOLD_SOLID_BREP('Body1',#5186);
#344=MANIFOLD_SOLID_BREP('Body1',#5187);
#345=FACE_BOUND('',#940,.T.);
#346=FACE_BOUND('',#941,.T.);
#347=FACE_BOUND('',#942,.T.);
#348=FACE_BOUND('',#943,.T.);
#349=FACE_BOUND('',#944,.T.);
#350=FACE_BOUND('',#945,.T.);
#351=FACE_BOUND('',#946,.T.);
#352=FACE_BOUND('',#948,.T.);
#353=FACE_BOUND('',#949,.T.);
#354=FACE_BOUND('',#950,.T.);
#355=FACE_BOUND('',#951,.T.);
#356=FACE_BOUND('',#952,.T.);
#357=FACE_BOUND('',#953,.T.);
#358=FACE_BOUND('',#954,.T.);
#359=FACE_BOUND('',#959,.T.);
#360=FACE_BOUND('',#963,.T.);
#361=FACE_BOUND('',#969,.T.);
#362=FACE_BOUND('',#970,.T.);
#363=FACE_BOUND('',#971,.T.);
#364=FACE_BOUND('',#973,.T.);
#365=FACE_BOUND('',#974,.T.);
#366=FACE_BOUND('',#975,.T.);
#367=FACE_BOUND('',#979,.T.);
#368=FACE_BOUND('',#984,.T.);
#369=FACE_BOUND('',#988,.T.);
#370=FACE_BOUND('',#990,.T.);
#371=FACE_BOUND('',#994,.T.);
#372=FACE_BOUND('',#996,.T.);
#373=FACE_BOUND('',#1000,.T.);
#374=FACE_BOUND('',#1002,.T.);
#375=FACE_BOUND('',#1015,.T.);
#376=FACE_BOUND('',#1035,.T.);
#377=FACE_BOUND('',#1036,.T.);
#378=FACE_BOUND('',#1037,.T.);
#379=FACE_BOUND('',#1038,.T.);
#380=FACE_BOUND('',#1039,.T.);
#381=FACE_BOUND('',#1046,.T.);
#382=FACE_BOUND('',#1048,.T.);
#383=FACE_BOUND('',#1050,.T.);
#384=FACE_BOUND('',#1052,.T.);
#385=FACE_BOUND('',#1053,.T.);
#386=FACE_BOUND('',#1054,.T.);
#387=FACE_BOUND('',#1055,.T.);
#388=FACE_BOUND('',#1056,.T.);
#389=FACE_BOUND('',#1058,.T.);
#390=FACE_BOUND('',#1059,.T.);
#391=FACE_BOUND('',#1060,.T.);
#392=FACE_BOUND('',#1061,.T.);
#393=FACE_BOUND('',#1062,.T.);
#394=FACE_BOUND('',#1065,.T.);
#395=FACE_BOUND('',#1068,.T.);
#396=FACE_BOUND('',#1071,.T.);
#397=FACE_BOUND('',#1074,.T.);
#398=FACE_BOUND('',#1081,.T.);
#399=FACE_BOUND('',#1085,.T.);
#400=FACE_BOUND('',#1086,.T.);
#401=FACE_BOUND('',#1087,.T.);
#402=FACE_BOUND('',#1088,.T.);
#403=FACE_BOUND('',#1089,.T.);
#404=FACE_BOUND('',#1091,.T.);
#405=FACE_BOUND('',#1092,.T.);
#406=FACE_BOUND('',#1093,.T.);
#407=FACE_BOUND('',#1094,.T.);
#408=FACE_BOUND('',#1095,.T.);
#409=FACE_BOUND('',#1101,.T.);
#410=FACE_BOUND('',#1104,.T.);
#411=FACE_BOUND('',#1109,.T.);
#412=FACE_BOUND('',#1114,.T.);
#413=FACE_BOUND('',#1142,.T.);
#414=FACE_BOUND('',#1145,.T.);
#415=FACE_BOUND('',#1148,.T.);
#416=FACE_BOUND('',#1151,.T.);
#417=FACE_BOUND('',#1154,.T.);
#418=FACE_BOUND('',#1170,.T.);
#419=FACE_BOUND('',#1187,.T.);
#420=FACE_BOUND('',#1196,.T.);
#421=FACE_BOUND('',#1199,.T.);
#422=FACE_BOUND('',#1207,.T.);
#423=FACE_BOUND('',#1209,.T.);
#424=FACE_BOUND('',#1214,.T.);
#425=FACE_BOUND('',#1216,.T.);
#426=FACE_BOUND('',#1218,.T.);
#427=FACE_BOUND('',#1220,.T.);
#428=FACE_BOUND('',#1230,.T.);
#429=FACE_BOUND('',#1237,.T.);
#430=FACE_BOUND('',#1239,.T.);
#431=FACE_BOUND('',#1241,.T.);
#432=FACE_BOUND('',#1291,.T.);
#433=FACE_BOUND('',#1293,.T.);
#434=FACE_BOUND('',#1302,.T.);
#435=FACE_BOUND('',#1309,.T.);
#436=FACE_BOUND('',#1324,.T.);
#437=PLANE('',#5477);
#438=PLANE('',#5478);
#439=PLANE('',#5479);
#440=PLANE('',#5480);
#441=PLANE('',#5481);
#442=PLANE('',#5482);
#443=PLANE('',#5493);
#444=PLANE('',#5500);
#445=PLANE('',#5501);
#446=PLANE('',#5502);
#447=PLANE('',#5503);
#448=PLANE('',#5504);
#449=PLANE('',#5505);
#450=PLANE('',#5506);
#451=PLANE('',#5511);
#452=PLANE('',#5512);
#453=PLANE('',#5517);
#454=PLANE('',#5520);
#455=PLANE('',#5528);
#456=PLANE('',#5529);
#457=PLANE('',#5537);
#458=PLANE('',#5538);
#459=PLANE('',#5546);
#460=PLANE('',#5547);
#461=PLANE('',#5552);
#462=PLANE('',#5557);
#463=PLANE('',#5558);
#464=PLANE('',#5559);
#465=PLANE('',#5562);
#466=PLANE('',#5563);
#467=PLANE('',#5564);
#468=PLANE('',#5565);
#469=PLANE('',#5568);
#470=PLANE('',#5574);
#471=PLANE('',#5578);
#472=PLANE('',#5582);
#473=PLANE('',#5586);
#474=PLANE('',#5587);
#475=PLANE('',#5595);
#476=PLANE('',#5600);
#477=PLANE('',#5605);
#478=PLANE('',#5614);
#479=PLANE('',#5631);
#480=PLANE('',#5637);
#481=PLANE('',#5638);
#482=PLANE('',#5643);
#483=PLANE('',#5648);
#484=PLANE('',#5653);
#485=PLANE('',#5658);
#486=PLANE('',#5671);
#487=PLANE('',#5678);
#488=PLANE('',#5679);
#489=PLANE('',#5695);
#490=PLANE('',#5698);
#491=PLANE('',#5710);
#492=PLANE('',#5719);
#493=PLANE('',#5752);
#494=PLANE('',#5757);
#495=PLANE('',#5762);
#496=PLANE('',#5767);
#497=PLANE('',#5772);
#498=PLANE('',#5777);
#499=PLANE('',#5786);
#500=PLANE('',#5790);
#501=PLANE('',#5791);
#502=PLANE('',#5793);
#503=PLANE('',#5798);
#504=PLANE('',#5801);
#505=PLANE('',#5806);
#506=PLANE('',#5815);
#507=PLANE('',#5816);
#508=PLANE('',#5817);
#509=PLANE('',#5818);
#510=PLANE('',#5819);
#511=PLANE('',#5820);
#512=PLANE('',#5821);
#513=PLANE('',#5822);
#514=PLANE('',#5823);
#515=PLANE('',#5825);
#516=PLANE('',#5833);
#517=PLANE('',#5839);
#518=PLANE('',#5840);
#519=PLANE('',#5841);
#520=PLANE('',#5842);
#521=PLANE('',#5843);
#522=PLANE('',#5844);
#523=PLANE('',#5845);
#524=PLANE('',#5846);
#525=PLANE('',#5847);
#526=PLANE('',#5849);
#527=PLANE('',#5857);
#528=PLANE('',#5869);
#529=PLANE('',#5870);
#530=PLANE('',#5896);
#531=PLANE('',#5901);
#532=PLANE('',#5907);
#533=PLANE('',#5908);
#534=PLANE('',#5916);
#535=PLANE('',#5917);
#536=PLANE('',#5919);
#537=PLANE('',#5923);
#538=PLANE('',#5930);
#539=PLANE('',#5931);
#540=PLANE('',#5933);
#541=PLANE('',#5935);
#542=PLANE('',#5936);
#543=PLANE('',#5937);
#544=PLANE('',#5938);
#545=PLANE('',#5939);
#546=PLANE('',#5940);
#547=PLANE('',#5941);
#548=PLANE('',#5942);
#549=PLANE('',#5948);
#550=PLANE('',#5953);
#551=PLANE('',#5957);
#552=PLANE('',#5961);
#553=PLANE('',#5962);
#554=PLANE('',#5963);
#555=PLANE('',#5964);
#556=PLANE('',#5965);
#557=PLANE('',#5966);
#558=PLANE('',#5967);
#559=PLANE('',#5968);
#560=PLANE('',#5969);
#561=PLANE('',#5970);
#562=PLANE('',#5971);
#563=PLANE('',#5972);
#564=PLANE('',#5973);
#565=PLANE('',#5974);
#566=PLANE('',#5975);
#567=PLANE('',#5976);
#568=PLANE('',#5977);
#569=PLANE('',#5978);
#570=PLANE('',#5979);
#571=PLANE('',#5980);
#572=PLANE('',#5981);
#573=PLANE('',#5982);
#574=PLANE('',#5983);
#575=PLANE('',#5984);
#576=PLANE('',#5985);
#577=PLANE('',#5986);
#578=PLANE('',#5987);
#579=PLANE('',#5988);
#580=PLANE('',#5989);
#581=PLANE('',#5990);
#582=PLANE('',#5991);
#583=PLANE('',#5992);
#584=PLANE('',#5993);
#585=PLANE('',#5994);
#586=PLANE('',#5995);
#587=PLANE('',#5996);
#588=PLANE('',#5997);
#589=PLANE('',#5998);
#590=PLANE('',#5999);
#591=PLANE('',#6000);
#592=PLANE('',#6001);
#593=PLANE('',#6002);
#594=PLANE('',#6003);
#595=PLANE('',#6004);
#596=PLANE('',#6005);
#597=PLANE('',#6006);
#598=PLANE('',#6007);
#599=PLANE('',#6008);
#600=PLANE('',#6009);
#601=PLANE('',#6010);
#602=PLANE('',#6012);
#603=PLANE('',#6013);
#604=PLANE('',#6014);
#605=PLANE('',#6015);
#606=PLANE('',#6016);
#607=PLANE('',#6017);
#608=PLANE('',#6018);
#609=PLANE('',#6019);
#610=PLANE('',#6027);
#611=PLANE('',#6039);
#612=PLANE('',#6046);
#613=PLANE('',#6047);
#614=PLANE('',#6048);
#615=PLANE('',#6050);
#616=PLANE('',#6051);
#617=PLANE('',#6052);
#618=PLANE('',#6053);
#619=PLANE('',#6058);
#620=PLANE('',#6059);
#621=PLANE('',#6060);
#622=PLANE('',#6061);
#623=FACE_OUTER_BOUND('',#928,.T.);
#624=FACE_OUTER_BOUND('',#929,.T.);
#625=FACE_OUTER_BOUND('',#930,.T.);
#626=FACE_OUTER_BOUND('',#931,.T.);
#627=FACE_OUTER_BOUND('',#932,.T.);
#628=FACE_OUTER_BOUND('',#933,.T.);
#629=FACE_OUTER_BOUND('',#934,.T.);
#630=FACE_OUTER_BOUND('',#935,.T.);
#631=FACE_OUTER_BOUND('',#936,.T.);
#632=FACE_OUTER_BOUND('',#937,.T.);
#633=FACE_OUTER_BOUND('',#938,.T.);
#634=FACE_OUTER_BOUND('',#939,.T.);
#635=FACE_OUTER_BOUND('',#947,.T.);
#636=FACE_OUTER_BOUND('',#955,.T.);
#637=FACE_OUTER_BOUND('',#956,.T.);
#638=FACE_OUTER_BOUND('',#957,.T.);
#639=FACE_OUTER_BOUND('',#958,.T.);
#640=FACE_OUTER_BOUND('',#960,.T.);
#641=FACE_OUTER_BOUND('',#961,.T.);
#642=FACE_OUTER_BOUND('',#962,.T.);
#643=FACE_OUTER_BOUND('',#964,.T.);
#644=FACE_OUTER_BOUND('',#965,.T.);
#645=FACE_OUTER_BOUND('',#966,.T.);
#646=FACE_OUTER_BOUND('',#967,.T.);
#647=FACE_OUTER_BOUND('',#968,.T.);
#648=FACE_OUTER_BOUND('',#972,.T.);
#649=FACE_OUTER_BOUND('',#976,.T.);
#650=FACE_OUTER_BOUND('',#977,.T.);
#651=FACE_OUTER_BOUND('',#978,.T.);
#652=FACE_OUTER_BOUND('',#980,.T.);
#653=FACE_OUTER_BOUND('',#981,.T.);
#654=FACE_OUTER_BOUND('',#982,.T.);
#655=FACE_OUTER_BOUND('',#983,.T.);
#656=FACE_OUTER_BOUND('',#985,.T.);
#657=FACE_OUTER_BOUND('',#986,.T.);
#658=FACE_OUTER_BOUND('',#987,.T.);
#659=FACE_OUTER_BOUND('',#989,.T.);
#660=FACE_OUTER_BOUND('',#991,.T.);
#661=FACE_OUTER_BOUND('',#992,.T.);
#662=FACE_OUTER_BOUND('',#993,.T.);
#663=FACE_OUTER_BOUND('',#995,.T.);
#664=FACE_OUTER_BOUND('',#997,.T.);
#665=FACE_OUTER_BOUND('',#998,.T.);
#666=FACE_OUTER_BOUND('',#999,.T.);
#667=FACE_OUTER_BOUND('',#1001,.T.);
#668=FACE_OUTER_BOUND('',#1003,.T.);
#669=FACE_OUTER_BOUND('',#1004,.T.);
#670=FACE_OUTER_BOUND('',#1005,.T.);
#671=FACE_OUTER_BOUND('',#1006,.T.);
#672=FACE_OUTER_BOUND('',#1007,.T.);
#673=FACE_OUTER_BOUND('',#1008,.T.);
#674=FACE_OUTER_BOUND('',#1009,.T.);
#675=FACE_OUTER_BOUND('',#1010,.T.);
#676=FACE_OUTER_BOUND('',#1011,.T.);
#677=FACE_OUTER_BOUND('',#1012,.T.);
#678=FACE_OUTER_BOUND('',#1013,.T.);
#679=FACE_OUTER_BOUND('',#1014,.T.);
#680=FACE_OUTER_BOUND('',#1016,.T.);
#681=FACE_OUTER_BOUND('',#1017,.T.);
#682=FACE_OUTER_BOUND('',#1018,.T.);
#683=FACE_OUTER_BOUND('',#1019,.T.);
#684=FACE_OUTER_BOUND('',#1020,.T.);
#685=FACE_OUTER_BOUND('',#1021,.T.);
#686=FACE_OUTER_BOUND('',#1022,.T.);
#687=FACE_OUTER_BOUND('',#1023,.T.);
#688=FACE_OUTER_BOUND('',#1024,.T.);
#689=FACE_OUTER_BOUND('',#1025,.T.);
#690=FACE_OUTER_BOUND('',#1026,.T.);
#691=FACE_OUTER_BOUND('',#1027,.T.);
#692=FACE_OUTER_BOUND('',#1028,.T.);
#693=FACE_OUTER_BOUND('',#1029,.T.);
#694=FACE_OUTER_BOUND('',#1030,.T.);
#695=FACE_OUTER_BOUND('',#1031,.T.);
#696=FACE_OUTER_BOUND('',#1032,.T.);
#697=FACE_OUTER_BOUND('',#1033,.T.);
#698=FACE_OUTER_BOUND('',#1034,.T.);
#699=FACE_OUTER_BOUND('',#1040,.T.);
#700=FACE_OUTER_BOUND('',#1041,.T.);
#701=FACE_OUTER_BOUND('',#1042,.T.);
#702=FACE_OUTER_BOUND('',#1043,.T.);
#703=FACE_OUTER_BOUND('',#1044,.T.);
#704=FACE_OUTER_BOUND('',#1045,.T.);
#705=FACE_OUTER_BOUND('',#1047,.T.);
#706=FACE_OUTER_BOUND('',#1049,.T.);
#707=FACE_OUTER_BOUND('',#1051,.T.);
#708=FACE_OUTER_BOUND('',#1057,.T.);
#709=FACE_OUTER_BOUND('',#1063,.T.);
#710=FACE_OUTER_BOUND('',#1064,.T.);
#711=FACE_OUTER_BOUND('',#1066,.T.);
#712=FACE_OUTER_BOUND('',#1067,.T.);
#713=FACE_OUTER_BOUND('',#1069,.T.);
#714=FACE_OUTER_BOUND('',#1070,.T.);
#715=FACE_OUTER_BOUND('',#1072,.T.);
#716=FACE_OUTER_BOUND('',#1073,.T.);
#717=FACE_OUTER_BOUND('',#1075,.T.);
#718=FACE_OUTER_BOUND('',#1076,.T.);
#719=FACE_OUTER_BOUND('',#1077,.T.);
#720=FACE_OUTER_BOUND('',#1078,.T.);
#721=FACE_OUTER_BOUND('',#1079,.T.);
#722=FACE_OUTER_BOUND('',#1080,.T.);
#723=FACE_OUTER_BOUND('',#1082,.T.);
#724=FACE_OUTER_BOUND('',#1083,.T.);
#725=FACE_OUTER_BOUND('',#1084,.T.);
#726=FACE_OUTER_BOUND('',#1090,.T.);
#727=FACE_OUTER_BOUND('',#1096,.T.);
#728=FACE_OUTER_BOUND('',#1097,.T.);
#729=FACE_OUTER_BOUND('',#1098,.T.);
#730=FACE_OUTER_BOUND('',#1099,.T.);
#731=FACE_OUTER_BOUND('',#1100,.T.);
#732=FACE_OUTER_BOUND('',#1102,.T.);
#733=FACE_OUTER_BOUND('',#1103,.T.);
#734=FACE_OUTER_BOUND('',#1105,.T.);
#735=FACE_OUTER_BOUND('',#1106,.T.);
#736=FACE_OUTER_BOUND('',#1107,.T.);
#737=FACE_OUTER_BOUND('',#1108,.T.);
#738=FACE_OUTER_BOUND('',#1110,.T.);
#739=FACE_OUTER_BOUND('',#1111,.T.);
#740=FACE_OUTER_BOUND('',#1112,.T.);
#741=FACE_OUTER_BOUND('',#1113,.T.);
#742=FACE_OUTER_BOUND('',#1115,.T.);
#743=FACE_OUTER_BOUND('',#1116,.T.);
#744=FACE_OUTER_BOUND('',#1117,.T.);
#745=FACE_OUTER_BOUND('',#1118,.T.);
#746=FACE_OUTER_BOUND('',#1119,.T.);
#747=FACE_OUTER_BOUND('',#1120,.T.);
#748=FACE_OUTER_BOUND('',#1121,.T.);
#749=FACE_OUTER_BOUND('',#1122,.T.);
#750=FACE_OUTER_BOUND('',#1123,.T.);
#751=FACE_OUTER_BOUND('',#1124,.T.);
#752=FACE_OUTER_BOUND('',#1125,.T.);
#753=FACE_OUTER_BOUND('',#1126,.T.);
#754=FACE_OUTER_BOUND('',#1127,.T.);
#755=FACE_OUTER_BOUND('',#1128,.T.);
#756=FACE_OUTER_BOUND('',#1129,.T.);
#757=FACE_OUTER_BOUND('',#1130,.T.);
#758=FACE_OUTER_BOUND('',#1131,.T.);
#759=FACE_OUTER_BOUND('',#1132,.T.);
#760=FACE_OUTER_BOUND('',#1133,.T.);
#761=FACE_OUTER_BOUND('',#1134,.T.);
#762=FACE_OUTER_BOUND('',#1135,.T.);
#763=FACE_OUTER_BOUND('',#1136,.T.);
#764=FACE_OUTER_BOUND('',#1137,.T.);
#765=FACE_OUTER_BOUND('',#1138,.T.);
#766=FACE_OUTER_BOUND('',#1139,.T.);
#767=FACE_OUTER_BOUND('',#1140,.T.);
#768=FACE_OUTER_BOUND('',#1141,.T.);
#769=FACE_OUTER_BOUND('',#1143,.T.);
#770=FACE_OUTER_BOUND('',#1144,.T.);
#771=FACE_OUTER_BOUND('',#1146,.T.);
#772=FACE_OUTER_BOUND('',#1147,.T.);
#773=FACE_OUTER_BOUND('',#1149,.T.);
#774=FACE_OUTER_BOUND('',#1150,.T.);
#775=FACE_OUTER_BOUND('',#1152,.T.);
#776=FACE_OUTER_BOUND('',#1153,.T.);
#777=FACE_OUTER_BOUND('',#1155,.T.);
#778=FACE_OUTER_BOUND('',#1156,.T.);
#779=FACE_OUTER_BOUND('',#1157,.T.);
#780=FACE_OUTER_BOUND('',#1158,.T.);
#781=FACE_OUTER_BOUND('',#1159,.T.);
#782=FACE_OUTER_BOUND('',#1160,.T.);
#783=FACE_OUTER_BOUND('',#1161,.T.);
#784=FACE_OUTER_BOUND('',#1162,.T.);
#785=FACE_OUTER_BOUND('',#1163,.T.);
#786=FACE_OUTER_BOUND('',#1164,.T.);
#787=FACE_OUTER_BOUND('',#1165,.T.);
#788=FACE_OUTER_BOUND('',#1166,.T.);
#789=FACE_OUTER_BOUND('',#1167,.T.);
#790=FACE_OUTER_BOUND('',#1168,.T.);
#791=FACE_OUTER_BOUND('',#1169,.T.);
#792=FACE_OUTER_BOUND('',#1171,.T.);
#793=FACE_OUTER_BOUND('',#1172,.T.);
#794=FACE_OUTER_BOUND('',#1173,.T.);
#795=FACE_OUTER_BOUND('',#1174,.T.);
#796=FACE_OUTER_BOUND('',#1175,.T.);
#797=FACE_OUTER_BOUND('',#1176,.T.);
#798=FACE_OUTER_BOUND('',#1177,.T.);
#799=FACE_OUTER_BOUND('',#1178,.T.);
#800=FACE_OUTER_BOUND('',#1179,.T.);
#801=FACE_OUTER_BOUND('',#1180,.T.);
#802=FACE_OUTER_BOUND('',#1181,.T.);
#803=FACE_OUTER_BOUND('',#1182,.T.);
#804=FACE_OUTER_BOUND('',#1183,.T.);
#805=FACE_OUTER_BOUND('',#1184,.T.);
#806=FACE_OUTER_BOUND('',#1185,.T.);
#807=FACE_OUTER_BOUND('',#1186,.T.);
#808=FACE_OUTER_BOUND('',#1188,.T.);
#809=FACE_OUTER_BOUND('',#1189,.T.);
#810=FACE_OUTER_BOUND('',#1190,.T.);
#811=FACE_OUTER_BOUND('',#1191,.T.);
#812=FACE_OUTER_BOUND('',#1192,.T.);
#813=FACE_OUTER_BOUND('',#1193,.T.);
#814=FACE_OUTER_BOUND('',#1194,.T.);
#815=FACE_OUTER_BOUND('',#1195,.T.);
#816=FACE_OUTER_BOUND('',#1197,.T.);
#817=FACE_OUTER_BOUND('',#1198,.T.);
#818=FACE_OUTER_BOUND('',#1200,.T.);
#819=FACE_OUTER_BOUND('',#1201,.T.);
#820=FACE_OUTER_BOUND('',#1202,.T.);
#821=FACE_OUTER_BOUND('',#1203,.T.);
#822=FACE_OUTER_BOUND('',#1204,.T.);
#823=FACE_OUTER_BOUND('',#1205,.T.);
#824=FACE_OUTER_BOUND('',#1206,.T.);
#825=FACE_OUTER_BOUND('',#1208,.T.);
#826=FACE_OUTER_BOUND('',#1210,.T.);
#827=FACE_OUTER_BOUND('',#1211,.T.);
#828=FACE_OUTER_BOUND('',#1212,.T.);
#829=FACE_OUTER_BOUND('',#1213,.T.);
#830=FACE_OUTER_BOUND('',#1215,.T.);
#831=FACE_OUTER_BOUND('',#1217,.T.);
#832=FACE_OUTER_BOUND('',#1219,.T.);
#833=FACE_OUTER_BOUND('',#1221,.T.);
#834=FACE_OUTER_BOUND('',#1222,.T.);
#835=FACE_OUTER_BOUND('',#1223,.T.);
#836=FACE_OUTER_BOUND('',#1224,.T.);
#837=FACE_OUTER_BOUND('',#1225,.T.);
#838=FACE_OUTER_BOUND('',#1226,.T.);
#839=FACE_OUTER_BOUND('',#1227,.T.);
#840=FACE_OUTER_BOUND('',#1228,.T.);
#841=FACE_OUTER_BOUND('',#1229,.T.);
#842=FACE_OUTER_BOUND('',#1231,.T.);
#843=FACE_OUTER_BOUND('',#1232,.T.);
#844=FACE_OUTER_BOUND('',#1233,.T.);
#845=FACE_OUTER_BOUND('',#1234,.T.);
#846=FACE_OUTER_BOUND('',#1235,.T.);
#847=FACE_OUTER_BOUND('',#1236,.T.);
#848=FACE_OUTER_BOUND('',#1238,.T.);
#849=FACE_OUTER_BOUND('',#1240,.T.);
#850=FACE_OUTER_BOUND('',#1242,.T.);
#851=FACE_OUTER_BOUND('',#1243,.T.);
#852=FACE_OUTER_BOUND('',#1244,.T.);
#853=FACE_OUTER_BOUND('',#1245,.T.);
#854=FACE_OUTER_BOUND('',#1246,.T.);
#855=FACE_OUTER_BOUND('',#1247,.T.);
#856=FACE_OUTER_BOUND('',#1248,.T.);
#857=FACE_OUTER_BOUND('',#1249,.T.);
#858=FACE_OUTER_BOUND('',#1250,.T.);
#859=FACE_OUTER_BOUND('',#1251,.T.);
#860=FACE_OUTER_BOUND('',#1252,.T.);
#861=FACE_OUTER_BOUND('',#1253,.T.);
#862=FACE_OUTER_BOUND('',#1254,.T.);
#863=FACE_OUTER_BOUND('',#1255,.T.);
#864=FACE_OUTER_BOUND('',#1256,.T.);
#865=FACE_OUTER_BOUND('',#1257,.T.);
#866=FACE_OUTER_BOUND('',#1258,.T.);
#867=FACE_OUTER_BOUND('',#1259,.T.);
#868=FACE_OUTER_BOUND('',#1260,.T.);
#869=FACE_OUTER_BOUND('',#1261,.T.);
#870=FACE_OUTER_BOUND('',#1262,.T.);
#871=FACE_OUTER_BOUND('',#1263,.T.);
#872=FACE_OUTER_BOUND('',#1264,.T.);
#873=FACE_OUTER_BOUND('',#1265,.T.);
#874=FACE_OUTER_BOUND('',#1266,.T.);
#875=FACE_OUTER_BOUND('',#1267,.T.);
#876=FACE_OUTER_BOUND('',#1268,.T.);
#877=FACE_OUTER_BOUND('',#1269,.T.);
#878=FACE_OUTER_BOUND('',#1270,.T.);
#879=FACE_OUTER_BOUND('',#1271,.T.);
#880=FACE_OUTER_BOUND('',#1272,.T.);
#881=FACE_OUTER_BOUND('',#1273,.T.);
#882=FACE_OUTER_BOUND('',#1274,.T.);
#883=FACE_OUTER_BOUND('',#1275,.T.);
#884=FACE_OUTER_BOUND('',#1276,.T.);
#885=FACE_OUTER_BOUND('',#1277,.T.);
#886=FACE_OUTER_BOUND('',#1278,.T.);
#887=FACE_OUTER_BOUND('',#1279,.T.);
#888=FACE_OUTER_BOUND('',#1280,.T.);
#889=FACE_OUTER_BOUND('',#1281,.T.);
#890=FACE_OUTER_BOUND('',#1282,.T.);
#891=FACE_OUTER_BOUND('',#1283,.T.);
#892=FACE_OUTER_BOUND('',#1284,.T.);
#893=FACE_OUTER_BOUND('',#1285,.T.);
#894=FACE_OUTER_BOUND('',#1286,.T.);
#895=FACE_OUTER_BOUND('',#1287,.T.);
#896=FACE_OUTER_BOUND('',#1288,.T.);
#897=FACE_OUTER_BOUND('',#1289,.T.);
#898=FACE_OUTER_BOUND('',#1290,.T.);
#899=FACE_OUTER_BOUND('',#1292,.T.);
#900=FACE_OUTER_BOUND('',#1294,.T.);
#901=FACE_OUTER_BOUND('',#1295,.T.);
#902=FACE_OUTER_BOUND('',#1296,.T.);
#903=FACE_OUTER_BOUND('',#1297,.T.);
#904=FACE_OUTER_BOUND('',#1298,.T.);
#905=FACE_OUTER_BOUND('',#1299,.T.);
#906=FACE_OUTER_BOUND('',#1300,.T.);
#907=FACE_OUTER_BOUND('',#1301,.T.);
#908=FACE_OUTER_BOUND('',#1303,.T.);
#909=FACE_OUTER_BOUND('',#1304,.T.);
#910=FACE_OUTER_BOUND('',#1305,.T.);
#911=FACE_OUTER_BOUND('',#1306,.T.);
#912=FACE_OUTER_BOUND('',#1307,.T.);
#913=FACE_OUTER_BOUND('',#1308,.T.);
#914=FACE_OUTER_BOUND('',#1310,.T.);
#915=FACE_OUTER_BOUND('',#1311,.T.);
#916=FACE_OUTER_BOUND('',#1312,.T.);
#917=FACE_OUTER_BOUND('',#1313,.T.);
#918=FACE_OUTER_BOUND('',#1314,.T.);
#919=FACE_OUTER_BOUND('',#1315,.T.);
#920=FACE_OUTER_BOUND('',#1316,.T.);
#921=FACE_OUTER_BOUND('',#1317,.T.);
#922=FACE_OUTER_BOUND('',#1318,.T.);
#923=FACE_OUTER_BOUND('',#1319,.T.);
#924=FACE_OUTER_BOUND('',#1320,.T.);
#925=FACE_OUTER_BOUND('',#1321,.T.);
#926=FACE_OUTER_BOUND('',#1322,.T.);
#927=FACE_OUTER_BOUND('',#1323,.T.);
#928=EDGE_LOOP('',(#3442,#3443,#3444,#3445));
#929=EDGE_LOOP('',(#3446,#3447,#3448,#3449));
#930=EDGE_LOOP('',(#3450,#3451,#3452,#3453));
#931=EDGE_LOOP('',(#3454,#3455,#3456,#3457));
#932=EDGE_LOOP('',(#3458,#3459,#3460,#3461));
#933=EDGE_LOOP('',(#3462,#3463,#3464,#3465));
#934=EDGE_LOOP('',(#3466,#3467,#3468,#3469));
#935=EDGE_LOOP('',(#3470,#3471,#3472,#3473));
#936=EDGE_LOOP('',(#3474,#3475,#3476,#3477));
#937=EDGE_LOOP('',(#3478,#3479,#3480,#3481));
#938=EDGE_LOOP('',(#3482,#3483,#3484,#3485));
#939=EDGE_LOOP('',(#3486,#3487,#3488,#3489));
#940=EDGE_LOOP('',(#3490));
#941=EDGE_LOOP('',(#3491));
#942=EDGE_LOOP('',(#3492));
#943=EDGE_LOOP('',(#3493));
#944=EDGE_LOOP('',(#3494));
#945=EDGE_LOOP('',(#3495));
#946=EDGE_LOOP('',(#3496));
#947=EDGE_LOOP('',(#3497,#3498,#3499,#3500));
#948=EDGE_LOOP('',(#3501));
#949=EDGE_LOOP('',(#3502));
#950=EDGE_LOOP('',(#3503));
#951=EDGE_LOOP('',(#3504));
#952=EDGE_LOOP('',(#3505));
#953=EDGE_LOOP('',(#3506));
#954=EDGE_LOOP('',(#3507));
#955=EDGE_LOOP('',(#3508,#3509,#3510,#3511));
#956=EDGE_LOOP('',(#3512,#3513,#3514,#3515));
#957=EDGE_LOOP('',(#3516,#3517,#3518,#3519));
#958=EDGE_LOOP('',(#3520));
#959=EDGE_LOOP('',(#3521));
#960=EDGE_LOOP('',(#3522,#3523,#3524,#3525));
#961=EDGE_LOOP('',(#3526,#3527,#3528,#3529));
#962=EDGE_LOOP('',(#3530));
#963=EDGE_LOOP('',(#3531));
#964=EDGE_LOOP('',(#3532,#3533,#3534,#3535));
#965=EDGE_LOOP('',(#3536,#3537,#3538,#3539));
#966=EDGE_LOOP('',(#3540,#3541,#3542,#3543));
#967=EDGE_LOOP('',(#3544,#3545,#3546,#3547));
#968=EDGE_LOOP('',(#3548,#3549,#3550,#3551));
#969=EDGE_LOOP('',(#3552));
#970=EDGE_LOOP('',(#3553));
#971=EDGE_LOOP('',(#3554));
#972=EDGE_LOOP('',(#3555,#3556,#3557,#3558));
#973=EDGE_LOOP('',(#3559));
#974=EDGE_LOOP('',(#3560));
#975=EDGE_LOOP('',(#3561));
#976=EDGE_LOOP('',(#3562,#3563,#3564,#3565));
#977=EDGE_LOOP('',(#3566));
#978=EDGE_LOOP('',(#3567));
#979=EDGE_LOOP('',(#3568));
#980=EDGE_LOOP('',(#3569,#3570,#3571,#3572));
#981=EDGE_LOOP('',(#3573));
#982=EDGE_LOOP('',(#3574,#3575,#3576,#3577));
#983=EDGE_LOOP('',(#3578));
#984=EDGE_LOOP('',(#3579));
#985=EDGE_LOOP('',(#3580,#3581,#3582,#3583));
#986=EDGE_LOOP('',(#3584,#3585,#3586,#3587));
#987=EDGE_LOOP('',(#3588));
#988=EDGE_LOOP('',(#3589));
#989=EDGE_LOOP('',(#3590));
#990=EDGE_LOOP('',(#3591));
#991=EDGE_LOOP('',(#3592,#3593,#3594,#3595));
#992=EDGE_LOOP('',(#3596,#3597,#3598,#3599));
#993=EDGE_LOOP('',(#3600));
#994=EDGE_LOOP('',(#3601));
#995=EDGE_LOOP('',(#3602));
#996=EDGE_LOOP('',(#3603));
#997=EDGE_LOOP('',(#3604,#3605,#3606,#3607));
#998=EDGE_LOOP('',(#3608,#3609,#3610,#3611));
#999=EDGE_LOOP('',(#3612));
#1000=EDGE_LOOP('',(#3613));
#1001=EDGE_LOOP('',(#3614));
#1002=EDGE_LOOP('',(#3615));
#1003=EDGE_LOOP('',(#3616,#3617,#3618,#3619));
#1004=EDGE_LOOP('',(#3620));
#1005=EDGE_LOOP('',(#3621,#3622,#3623,#3624,#3625));
#1006=EDGE_LOOP('',(#3626));
#1007=EDGE_LOOP('',(#3627,#3628,#3629,#3630,#3631,#3632,#3633));
#1008=EDGE_LOOP('',(#3634,#3635,#3636,#3637,#3638,#3639,#3640));
#1009=EDGE_LOOP('',(#3641,#3642,#3643,#3644));
#1010=EDGE_LOOP('',(#3645,#3646,#3647,#3648,#3649));
#1011=EDGE_LOOP('',(#3650,#3651,#3652,#3653,#3654));
#1012=EDGE_LOOP('',(#3655,#3656,#3657,#3658));
#1013=EDGE_LOOP('',(#3659,#3660,#3661,#3662,#3663));
#1014=EDGE_LOOP('',(#3664));
#1015=EDGE_LOOP('',(#3665));
#1016=EDGE_LOOP('',(#3666,#3667,#3668,#3669,#3670,#3671));
#1017=EDGE_LOOP('',(#3672,#3673,#3674,#3675));
#1018=EDGE_LOOP('',(#3676));
#1019=EDGE_LOOP('',(#3677,#3678,#3679,#3680));
#1020=EDGE_LOOP('',(#3681));
#1021=EDGE_LOOP('',(#3682,#3683,#3684,#3685));
#1022=EDGE_LOOP('',(#3686));
#1023=EDGE_LOOP('',(#3687,#3688,#3689,#3690));
#1024=EDGE_LOOP('',(#3691));
#1025=EDGE_LOOP('',(#3692,#3693));
#1026=EDGE_LOOP('',(#3694,#3695,#3696,#3697));
#1027=EDGE_LOOP('',(#3698,#3699,#3700,#3701));
#1028=EDGE_LOOP('',(#3702,#3703));
#1029=EDGE_LOOP('',(#3704,#3705,#3706,#3707));
#1030=EDGE_LOOP('',(#3708,#3709));
#1031=EDGE_LOOP('',(#3710,#3711,#3712,#3713));
#1032=EDGE_LOOP('',(#3714,#3715));
#1033=EDGE_LOOP('',(#3716,#3717,#3718,#3719,#3720,#3721,#3722,#3723,#3724,
#3725,#3726,#3727,#3728,#3729,#3730,#3731,#3732,#3733,#3734,#3735));
#1034=EDGE_LOOP('',(#3736));
#1035=EDGE_LOOP('',(#3737,#3738,#3739,#3740,#3741,#3742,#3743,#3744,#3745));
#1036=EDGE_LOOP('',(#3746));
#1037=EDGE_LOOP('',(#3747));
#1038=EDGE_LOOP('',(#3748));
#1039=EDGE_LOOP('',(#3749));
#1040=EDGE_LOOP('',(#3750,#3751,#3752,#3753));
#1041=EDGE_LOOP('',(#3754,#3755,#3756,#3757));
#1042=EDGE_LOOP('',(#3758,#3759,#3760,#3761));
#1043=EDGE_LOOP('',(#3762,#3763,#3764,#3765));
#1044=EDGE_LOOP('',(#3766,#3767,#3768,#3769));
#1045=EDGE_LOOP('',(#3770));
#1046=EDGE_LOOP('',(#3771));
#1047=EDGE_LOOP('',(#3772,#3773,#3774,#3775));
#1048=EDGE_LOOP('',(#3776,#3777));
#1049=EDGE_LOOP('',(#3778,#3779,#3780,#3781));
#1050=EDGE_LOOP('',(#3782,#3783));
#1051=EDGE_LOOP('',(#3784));
#1052=EDGE_LOOP('',(#3785));
#1053=EDGE_LOOP('',(#3786));
#1054=EDGE_LOOP('',(#3787));
#1055=EDGE_LOOP('',(#3788));
#1056=EDGE_LOOP('',(#3789));
#1057=EDGE_LOOP('',(#3790));
#1058=EDGE_LOOP('',(#3791));
#1059=EDGE_LOOP('',(#3792));
#1060=EDGE_LOOP('',(#3793));
#1061=EDGE_LOOP('',(#3794));
#1062=EDGE_LOOP('',(#3795));
#1063=EDGE_LOOP('',(#3796,#3797,#3798,#3799));
#1064=EDGE_LOOP('',(#3800));
#1065=EDGE_LOOP('',(#3801));
#1066=EDGE_LOOP('',(#3802,#3803,#3804,#3805));
#1067=EDGE_LOOP('',(#3806));
#1068=EDGE_LOOP('',(#3807));
#1069=EDGE_LOOP('',(#3808,#3809,#3810,#3811));
#1070=EDGE_LOOP('',(#3812));
#1071=EDGE_LOOP('',(#3813));
#1072=EDGE_LOOP('',(#3814,#3815,#3816,#3817));
#1073=EDGE_LOOP('',(#3818));
#1074=EDGE_LOOP('',(#3819));
#1075=EDGE_LOOP('',(#3820,#3821,#3822,#3823));
#1076=EDGE_LOOP('',(#3824,#3825,#3826,#3827));
#1077=EDGE_LOOP('',(#3828,#3829,#3830,#3831));
#1078=EDGE_LOOP('',(#3832,#3833,#3834,#3835));
#1079=EDGE_LOOP('',(#3836,#3837,#3838,#3839));
#1080=EDGE_LOOP('',(#3840));
#1081=EDGE_LOOP('',(#3841));
#1082=EDGE_LOOP('',(#3842,#3843,#3844,#3845));
#1083=EDGE_LOOP('',(#3846,#3847,#3848,#3849));
#1084=EDGE_LOOP('',(#3850));
#1085=EDGE_LOOP('',(#3851));
#1086=EDGE_LOOP('',(#3852));
#1087=EDGE_LOOP('',(#3853));
#1088=EDGE_LOOP('',(#3854));
#1089=EDGE_LOOP('',(#3855));
#1090=EDGE_LOOP('',(#3856));
#1091=EDGE_LOOP('',(#3857));
#1092=EDGE_LOOP('',(#3858));
#1093=EDGE_LOOP('',(#3859));
#1094=EDGE_LOOP('',(#3860));
#1095=EDGE_LOOP('',(#3861));
#1096=EDGE_LOOP('',(#3862,#3863,#3864,#3865,#3866,#3867));
#1097=EDGE_LOOP('',(#3868,#3869,#3870,#3871,#3872));
#1098=EDGE_LOOP('',(#3873,#3874,#3875,#3876));
#1099=EDGE_LOOP('',(#3877,#3878,#3879,#3880));
#1100=EDGE_LOOP('',(#3881));
#1101=EDGE_LOOP('',(#3882));
#1102=EDGE_LOOP('',(#3883,#3884,#3885,#3886,#3887));
#1103=EDGE_LOOP('',(#3888));
#1104=EDGE_LOOP('',(#3889));
#1105=EDGE_LOOP('',(#3890,#3891,#3892,#3893));
#1106=EDGE_LOOP('',(#3894,#3895,#3896,#3897,#3898,#3899));
#1107=EDGE_LOOP('',(#3900,#3901,#3902,#3903,#3904));
#1108=EDGE_LOOP('',(#3905));
#1109=EDGE_LOOP('',(#3906));
#1110=EDGE_LOOP('',(#3907,#3908,#3909,#3910));
#1111=EDGE_LOOP('',(#3911,#3912,#3913,#3914));
#1112=EDGE_LOOP('',(#3915,#3916,#3917,#3918));
#1113=EDGE_LOOP('',(#3919));
#1114=EDGE_LOOP('',(#3920));
#1115=EDGE_LOOP('',(#3921,#3922,#3923,#3924,#3925));
#1116=EDGE_LOOP('',(#3926,#3927));
#1117=EDGE_LOOP('',(#3928,#3929));
#1118=EDGE_LOOP('',(#3930,#3931));
#1119=EDGE_LOOP('',(#3932,#3933));
#1120=EDGE_LOOP('',(#3934,#3935));
#1121=EDGE_LOOP('',(#3936,#3937));
#1122=EDGE_LOOP('',(#3938,#3939));
#1123=EDGE_LOOP('',(#3940,#3941));
#1124=EDGE_LOOP('',(#3942,#3943,#3944,#3945));
#1125=EDGE_LOOP('',(#3946,#3947,#3948,#3949,#3950,#3951,#3952,#3953,#3954,
#3955,#3956,#3957,#3958,#3959,#3960,#3961,#3962,#3963,#3964,#3965));
#1126=EDGE_LOOP('',(#3966,#3967,#3968,#3969));
#1127=EDGE_LOOP('',(#3970,#3971,#3972,#3973));
#1128=EDGE_LOOP('',(#3974,#3975,#3976,#3977));
#1129=EDGE_LOOP('',(#3978,#3979,#3980,#3981));
#1130=EDGE_LOOP('',(#3982,#3983,#3984,#3985));
#1131=EDGE_LOOP('',(#3986,#3987,#3988,#3989,#3990,#3991));
#1132=EDGE_LOOP('',(#3992,#3993,#3994,#3995));
#1133=EDGE_LOOP('',(#3996,#3997,#3998,#3999));
#1134=EDGE_LOOP('',(#4000,#4001,#4002,#4003));
#1135=EDGE_LOOP('',(#4004,#4005,#4006,#4007));
#1136=EDGE_LOOP('',(#4008,#4009,#4010,#4011));
#1137=EDGE_LOOP('',(#4012,#4013,#4014,#4015));
#1138=EDGE_LOOP('',(#4016,#4017,#4018,#4019,#4020,#4021,#4022,#4023,#4024,
#4025,#4026,#4027,#4028,#4029,#4030,#4031,#4032,#4033,#4034,#4035));
#1139=EDGE_LOOP('',(#4036,#4037,#4038,#4039));
#1140=EDGE_LOOP('',(#4040,#4041,#4042,#4043));
#1141=EDGE_LOOP('',(#4044));
#1142=EDGE_LOOP('',(#4045));
#1143=EDGE_LOOP('',(#4046,#4047,#4048,#4049));
#1144=EDGE_LOOP('',(#4050));
#1145=EDGE_LOOP('',(#4051));
#1146=EDGE_LOOP('',(#4052,#4053,#4054,#4055));
#1147=EDGE_LOOP('',(#4056));
#1148=EDGE_LOOP('',(#4057));
#1149=EDGE_LOOP('',(#4058,#4059,#4060,#4061));
#1150=EDGE_LOOP('',(#4062));
#1151=EDGE_LOOP('',(#4063));
#1152=EDGE_LOOP('',(#4064,#4065,#4066,#4067));
#1153=EDGE_LOOP('',(#4068));
#1154=EDGE_LOOP('',(#4069));
#1155=EDGE_LOOP('',(#4070,#4071,#4072,#4073));
#1156=EDGE_LOOP('',(#4074,#4075,#4076,#4077));
#1157=EDGE_LOOP('',(#4078,#4079,#4080,#4081));
#1158=EDGE_LOOP('',(#4082,#4083,#4084,#4085));
#1159=EDGE_LOOP('',(#4086,#4087,#4088,#4089));
#1160=EDGE_LOOP('',(#4090,#4091,#4092,#4093));
#1161=EDGE_LOOP('',(#4094,#4095,#4096,#4097));
#1162=EDGE_LOOP('',(#4098,#4099,#4100,#4101,#4102,#4103));
#1163=EDGE_LOOP('',(#4104,#4105,#4106,#4107,#4108,#4109));
#1164=EDGE_LOOP('',(#4110));
#1165=EDGE_LOOP('',(#4111));
#1166=EDGE_LOOP('',(#4112,#4113,#4114,#4115));
#1167=EDGE_LOOP('',(#4116,#4117,#4118,#4119));
#1168=EDGE_LOOP('',(#4120,#4121,#4122,#4123));
#1169=EDGE_LOOP('',(#4124));
#1170=EDGE_LOOP('',(#4125));
#1171=EDGE_LOOP('',(#4126,#4127,#4128,#4129));
#1172=EDGE_LOOP('',(#4130,#4131,#4132,#4133));
#1173=EDGE_LOOP('',(#4134,#4135,#4136,#4137));
#1174=EDGE_LOOP('',(#4138,#4139,#4140,#4141));
#1175=EDGE_LOOP('',(#4142,#4143,#4144,#4145));
#1176=EDGE_LOOP('',(#4146,#4147,#4148,#4149));
#1177=EDGE_LOOP('',(#4150,#4151,#4152,#4153));
#1178=EDGE_LOOP('',(#4154,#4155,#4156,#4157));
#1179=EDGE_LOOP('',(#4158,#4159,#4160,#4161,#4162,#4163));
#1180=EDGE_LOOP('',(#4164,#4165,#4166,#4167,#4168,#4169));
#1181=EDGE_LOOP('',(#4170));
#1182=EDGE_LOOP('',(#4171));
#1183=EDGE_LOOP('',(#4172,#4173,#4174,#4175));
#1184=EDGE_LOOP('',(#4176,#4177,#4178,#4179));
#1185=EDGE_LOOP('',(#4180,#4181,#4182,#4183));
#1186=EDGE_LOOP('',(#4184));
#1187=EDGE_LOOP('',(#4185));
#1188=EDGE_LOOP('',(#4186,#4187,#4188,#4189));
#1189=EDGE_LOOP('',(#4190,#4191,#4192,#4193));
#1190=EDGE_LOOP('',(#4194,#4195,#4196,#4197));
#1191=EDGE_LOOP('',(#4198,#4199,#4200,#4201));
#1192=EDGE_LOOP('',(#4202,#4203,#4204,#4205));
#1193=EDGE_LOOP('',(#4206,#4207,#4208));
#1194=EDGE_LOOP('',(#4209,#4210,#4211));
#1195=EDGE_LOOP('',(#4212));
#1196=EDGE_LOOP('',(#4213));
#1197=EDGE_LOOP('',(#4214,#4215,#4216,#4217));
#1198=EDGE_LOOP('',(#4218));
#1199=EDGE_LOOP('',(#4219));
#1200=EDGE_LOOP('',(#4220,#4221,#4222,#4223));
#1201=EDGE_LOOP('',(#4224,#4225,#4226,#4227));
#1202=EDGE_LOOP('',(#4228));
#1203=EDGE_LOOP('',(#4229));
#1204=EDGE_LOOP('',(#4230,#4231,#4232,#4233));
#1205=EDGE_LOOP('',(#4234,#4235,#4236,#4237));
#1206=EDGE_LOOP('',(#4238));
#1207=EDGE_LOOP('',(#4239));
#1208=EDGE_LOOP('',(#4240));
#1209=EDGE_LOOP('',(#4241));
#1210=EDGE_LOOP('',(#4242,#4243));
#1211=EDGE_LOOP('',(#4244,#4245,#4246,#4247,#4248,#4249,#4250,#4251,#4252));
#1212=EDGE_LOOP('',(#4253,#4254));
#1213=EDGE_LOOP('',(#4255,#4256,#4257,#4258));
#1214=EDGE_LOOP('',(#4259,#4260,#4261,#4262,#4263));
#1215=EDGE_LOOP('',(#4264,#4265,#4266,#4267));
#1216=EDGE_LOOP('',(#4268,#4269));
#1217=EDGE_LOOP('',(#4270));
#1218=EDGE_LOOP('',(#4271));
#1219=EDGE_LOOP('',(#4272));
#1220=EDGE_LOOP('',(#4273));
#1221=EDGE_LOOP('',(#4274));
#1222=EDGE_LOOP('',(#4275,#4276,#4277,#4278));
#1223=EDGE_LOOP('',(#4279,#4280,#4281,#4282));
#1224=EDGE_LOOP('',(#4283,#4284,#4285,#4286));
#1225=EDGE_LOOP('',(#4287,#4288,#4289,#4290));
#1226=EDGE_LOOP('',(#4291,#4292,#4293,#4294));
#1227=EDGE_LOOP('',(#4295,#4296,#4297,#4298));
#1228=EDGE_LOOP('',(#4299,#4300,#4301,#4302,#4303,#4304));
#1229=EDGE_LOOP('',(#4305));
#1230=EDGE_LOOP('',(#4306,#4307,#4308,#4309,#4310,#4311));
#1231=EDGE_LOOP('',(#4312,#4313,#4314,#4315));
#1232=EDGE_LOOP('',(#4316,#4317,#4318,#4319));
#1233=EDGE_LOOP('',(#4320,#4321));
#1234=EDGE_LOOP('',(#4322,#4323,#4324,#4325,#4326,#4327,#4328,#4329,#4330));
#1235=EDGE_LOOP('',(#4331,#4332,#4333));
#1236=EDGE_LOOP('',(#4334,#4335,#4336,#4337));
#1237=EDGE_LOOP('',(#4338,#4339));
#1238=EDGE_LOOP('',(#4340));
#1239=EDGE_LOOP('',(#4341));
#1240=EDGE_LOOP('',(#4342,#4343,#4344,#4345));
#1241=EDGE_LOOP('',(#4346,#4347,#4348,#4349));
#1242=EDGE_LOOP('',(#4350,#4351,#4352,#4353));
#1243=EDGE_LOOP('',(#4354,#4355,#4356,#4357));
#1244=EDGE_LOOP('',(#4358,#4359,#4360,#4361));
#1245=EDGE_LOOP('',(#4362,#4363,#4364,#4365));
#1246=EDGE_LOOP('',(#4366,#4367,#4368,#4369));
#1247=EDGE_LOOP('',(#4370,#4371,#4372,#4373));
#1248=EDGE_LOOP('',(#4374,#4375,#4376,#4377));
#1249=EDGE_LOOP('',(#4378,#4379,#4380,#4381));
#1250=EDGE_LOOP('',(#4382,#4383,#4384,#4385));
#1251=EDGE_LOOP('',(#4386,#4387,#4388,#4389));
#1252=EDGE_LOOP('',(#4390,#4391,#4392,#4393));
#1253=EDGE_LOOP('',(#4394,#4395,#4396,#4397));
#1254=EDGE_LOOP('',(#4398,#4399,#4400,#4401));
#1255=EDGE_LOOP('',(#4402,#4403,#4404,#4405));
#1256=EDGE_LOOP('',(#4406,#4407,#4408,#4409));
#1257=EDGE_LOOP('',(#4410,#4411,#4412,#4413));
#1258=EDGE_LOOP('',(#4414,#4415,#4416,#4417));
#1259=EDGE_LOOP('',(#4418,#4419,#4420,#4421));
#1260=EDGE_LOOP('',(#4422,#4423,#4424,#4425));
#1261=EDGE_LOOP('',(#4426,#4427,#4428,#4429));
#1262=EDGE_LOOP('',(#4430,#4431,#4432,#4433));
#1263=EDGE_LOOP('',(#4434,#4435,#4436,#4437));
#1264=EDGE_LOOP('',(#4438,#4439,#4440,#4441));
#1265=EDGE_LOOP('',(#4442,#4443,#4444,#4445));
#1266=EDGE_LOOP('',(#4446,#4447,#4448,#4449));
#1267=EDGE_LOOP('',(#4450,#4451,#4452,#4453));
#1268=EDGE_LOOP('',(#4454,#4455,#4456,#4457));
#1269=EDGE_LOOP('',(#4458,#4459,#4460,#4461));
#1270=EDGE_LOOP('',(#4462,#4463,#4464,#4465));
#1271=EDGE_LOOP('',(#4466,#4467,#4468,#4469));
#1272=EDGE_LOOP('',(#4470,#4471,#4472,#4473));
#1273=EDGE_LOOP('',(#4474,#4475,#4476,#4477));
#1274=EDGE_LOOP('',(#4478,#4479,#4480,#4481));
#1275=EDGE_LOOP('',(#4482,#4483,#4484,#4485));
#1276=EDGE_LOOP('',(#4486,#4487,#4488,#4489));
#1277=EDGE_LOOP('',(#4490,#4491,#4492,#4493));
#1278=EDGE_LOOP('',(#4494,#4495,#4496,#4497));
#1279=EDGE_LOOP('',(#4498,#4499,#4500,#4501));
#1280=EDGE_LOOP('',(#4502,#4503,#4504,#4505));
#1281=EDGE_LOOP('',(#4506,#4507,#4508,#4509));
#1282=EDGE_LOOP('',(#4510,#4511,#4512,#4513));
#1283=EDGE_LOOP('',(#4514,#4515,#4516,#4517));
#1284=EDGE_LOOP('',(#4518,#4519,#4520,#4521));
#1285=EDGE_LOOP('',(#4522,#4523,#4524,#4525));
#1286=EDGE_LOOP('',(#4526,#4527,#4528,#4529));
#1287=EDGE_LOOP('',(#4530,#4531,#4532,#4533));
#1288=EDGE_LOOP('',(#4534,#4535,#4536,#4537));
#1289=EDGE_LOOP('',(#4538,#4539,#4540,#4541));
#1290=EDGE_LOOP('',(#4542,#4543,#4544,#4545,#4546,#4547,#4548,#4549,#4550,
#4551,#4552,#4553,#4554,#4555,#4556,#4557,#4558,#4559,#4560,#4561,#4562,
#4563,#4564,#4565,#4566,#4567,#4568,#4569,#4570,#4571,#4572,#4573,#4574,
#4575,#4576,#4577,#4578,#4579,#4580,#4581,#4582,#4583,#4584,#4585,#4586,
#4587,#4588,#4589));
#1291=EDGE_LOOP('',(#4590));
#1292=EDGE_LOOP('',(#4591,#4592,#4593,#4594,#4595,#4596,#4597,#4598,#4599,
#4600,#4601,#4602,#4603,#4604,#4605,#4606,#4607,#4608,#4609,#4610,#4611,
#4612,#4613,#4614,#4615,#4616,#4617,#4618,#4619,#4620,#4621,#4622,#4623,
#4624,#4625,#4626,#4627,#4628,#4629,#4630,#4631,#4632,#4633,#4634,#4635,
#4636,#4637,#4638));
#1293=EDGE_LOOP('',(#4639));
#1294=EDGE_LOOP('',(#4640,#4641,#4642,#4643));
#1295=EDGE_LOOP('',(#4644,#4645,#4646,#4647));
#1296=EDGE_LOOP('',(#4648,#4649,#4650,#4651));
#1297=EDGE_LOOP('',(#4652,#4653,#4654,#4655));
#1298=EDGE_LOOP('',(#4656,#4657,#4658,#4659));
#1299=EDGE_LOOP('',(#4660,#4661,#4662,#4663));
#1300=EDGE_LOOP('',(#4664,#4665,#4666,#4667,#4668,#4669));
#1301=EDGE_LOOP('',(#4670));
#1302=EDGE_LOOP('',(#4671,#4672,#4673,#4674,#4675,#4676));
#1303=EDGE_LOOP('',(#4677,#4678,#4679,#4680));
#1304=EDGE_LOOP('',(#4681,#4682,#4683,#4684));
#1305=EDGE_LOOP('',(#4685,#4686,#4687,#4688));
#1306=EDGE_LOOP('',(#4689));
#1307=EDGE_LOOP('',(#4690,#4691,#4692,#4693));
#1308=EDGE_LOOP('',(#4694,#4695,#4696,#4697,#4698,#4699,#4700));
#1309=EDGE_LOOP('',(#4701));
#1310=EDGE_LOOP('',(#4702,#4703,#4704,#4705,#4706));
#1311=EDGE_LOOP('',(#4707));
#1312=EDGE_LOOP('',(#4708,#4709));
#1313=EDGE_LOOP('',(#4710,#4711,#4712,#4713,#4714));
#1314=EDGE_LOOP('',(#4715,#4716,#4717,#4718,#4719,#4720));
#1315=EDGE_LOOP('',(#4721,#4722,#4723,#4724,#4725));
#1316=EDGE_LOOP('',(#4726,#4727,#4728,#4729,#4730));
#1317=EDGE_LOOP('',(#4731,#4732,#4733,#4734,#4735,#4736));
#1318=EDGE_LOOP('',(#4737,#4738,#4739,#4740));
#1319=EDGE_LOOP('',(#4741,#4742,#4743,#4744,#4745));
#1320=EDGE_LOOP('',(#4746,#4747,#4748,#4749));
#1321=EDGE_LOOP('',(#4750,#4751,#4752,#4753));
#1322=EDGE_LOOP('',(#4754,#4755,#4756,#4757,#4758));
#1323=EDGE_LOOP('',(#4759,#4760,#4761,#4762));
#1324=EDGE_LOOP('',(#4763));
#1325=LINE('',#7682,#1708);
#1326=LINE('',#7688,#1709);
#1327=LINE('',#7694,#1710);
#1328=LINE('',#7700,#1711);
#1329=LINE('',#7706,#1712);
#1330=LINE('',#7712,#1713);
#1331=LINE('',#7718,#1714);
#1332=LINE('',#7723,#1715);
#1333=LINE('',#7725,#1716);
#1334=LINE('',#7727,#1717);
#1335=LINE('',#7728,#1718);
#1336=LINE('',#7731,#1719);
#1337=LINE('',#7733,#1720);
#1338=LINE('',#7734,#1721);
#1339=LINE('',#7737,#1722);
#1340=LINE('',#7739,#1723);
#1341=LINE('',#7740,#1724);
#1342=LINE('',#7742,#1725);
#1343=LINE('',#7743,#1726);
#1344=LINE('',#7751,#1727);
#1345=LINE('',#7757,#1728);
#1346=LINE('',#7763,#1729);
#1347=LINE('',#7770,#1730);
#1348=LINE('',#7776,#1731);
#1349=LINE('',#7782,#1732);
#1350=LINE('',#7784,#1733);
#1351=LINE('',#7786,#1734);
#1352=LINE('',#7787,#1735);
#1353=LINE('',#7790,#1736);
#1354=LINE('',#7792,#1737);
#1355=LINE('',#7793,#1738);
#1356=LINE('',#7796,#1739);
#1357=LINE('',#7798,#1740);
#1358=LINE('',#7799,#1741);
#1359=LINE('',#7801,#1742);
#1360=LINE('',#7802,#1743);
#1361=LINE('',#7810,#1744);
#1362=LINE('',#7820,#1745);
#1363=LINE('',#7826,#1746);
#1364=LINE('',#7833,#1747);
#1365=LINE('',#7839,#1748);
#1366=LINE('',#7848,#1749);
#1367=LINE('',#7854,#1750);
#1368=LINE('',#7863,#1751);
#1369=LINE('',#7869,#1752);
#1370=LINE('',#7878,#1753);
#1371=LINE('',#7885,#1754);
#1372=LINE('',#7893,#1755);
#1373=LINE('',#7894,#1756);
#1374=LINE('',#7896,#1757);
#1375=LINE('',#7898,#1758);
#1376=LINE('',#7899,#1759);
#1377=LINE('',#7903,#1760);
#1378=LINE('',#7905,#1761);
#1379=LINE('',#7907,#1762);
#1380=LINE('',#7912,#1763);
#1381=LINE('',#7913,#1764);
#1382=LINE('',#7915,#1765);
#1383=LINE('',#7916,#1766);
#1384=LINE('',#7918,#1767);
#1385=LINE('',#7920,#1768);
#1386=LINE('',#7924,#1769);
#1387=LINE('',#7968,#1770);
#1388=LINE('',#8010,#1771);
#1389=LINE('',#8017,#1772);
#1390=LINE('',#8024,#1773);
#1391=LINE('',#8031,#1774);
#1392=LINE('',#8041,#1775);
#1393=LINE('',#8044,#1776);
#1394=LINE('',#8048,#1777);
#1395=LINE('',#8052,#1778);
#1396=LINE('',#8059,#1779);
#1397=LINE('',#8063,#1780);
#1398=LINE('',#8070,#1781);
#1399=LINE('',#8074,#1782);
#1400=LINE('',#8082,#1783);
#1401=LINE('',#8102,#1784);
#1402=LINE('',#8106,#1785);
#1403=LINE('',#8110,#1786);
#1404=LINE('',#8114,#1787);
#1405=LINE('',#8119,#1788);
#1406=LINE('',#8126,#1789);
#1407=LINE('',#8130,#1790);
#1408=LINE('',#8139,#1791);
#1409=LINE('',#8148,#1792);
#1410=LINE('',#8157,#1793);
#1411=LINE('',#8166,#1794);
#1412=LINE('',#8174,#1795);
#1413=LINE('',#8178,#1796);
#1414=LINE('',#8182,#1797);
#1415=LINE('',#8186,#1798);
#1416=LINE('',#8191,#1799);
#1417=LINE('',#8199,#1800);
#1418=LINE('',#8204,#1801);
#1419=LINE('',#8222,#1802);
#1420=LINE('',#8228,#1803);
#1421=LINE('',#8232,#1804);
#1422=LINE('',#8238,#1805);
#1423=LINE('',#8243,#1806);
#1424=LINE('',#8258,#1807);
#1425=LINE('',#8267,#1808);
#1426=LINE('',#8271,#1809);
#1427=LINE('',#8275,#1810);
#1428=LINE('',#8278,#1811);
#1429=LINE('',#8431,#1812);
#1430=LINE('',#8727,#1813);
#1431=LINE('',#8769,#1814);
#1432=LINE('',#8774,#1815);
#1433=LINE('',#8783,#1816);
#1434=LINE('',#8788,#1817);
#1435=LINE('',#8798,#1818);
#1436=LINE('',#8800,#1819);
#1437=LINE('',#8802,#1820);
#1438=LINE('',#8803,#1821);
#1439=LINE('',#8806,#1822);
#1440=LINE('',#8808,#1823);
#1441=LINE('',#8809,#1824);
#1442=LINE('',#8812,#1825);
#1443=LINE('',#8814,#1826);
#1444=LINE('',#8815,#1827);
#1445=LINE('',#8818,#1828);
#1446=LINE('',#8820,#1829);
#1447=LINE('',#8821,#1830);
#1448=LINE('',#8824,#1831);
#1449=LINE('',#8826,#1832);
#1450=LINE('',#8827,#1833);
#1451=LINE('',#8829,#1834);
#1452=LINE('',#8830,#1835);
#1453=LINE('',#8842,#1836);
#1454=LINE('',#8846,#1837);
#1455=LINE('',#8850,#1838);
#1456=LINE('',#8857,#1839);
#1457=LINE('',#8859,#1840);
#1458=LINE('',#8864,#1841);
#1459=LINE('',#8866,#1842);
#1460=LINE('',#8868,#1843);
#1461=LINE('',#8869,#1844);
#1462=LINE('',#8872,#1845);
#1463=LINE('',#8874,#1846);
#1464=LINE('',#8875,#1847);
#1465=LINE('',#8878,#1848);
#1466=LINE('',#8880,#1849);
#1467=LINE('',#8881,#1850);
#1468=LINE('',#8884,#1851);
#1469=LINE('',#8886,#1852);
#1470=LINE('',#8887,#1853);
#1471=LINE('',#8890,#1854);
#1472=LINE('',#8892,#1855);
#1473=LINE('',#8893,#1856);
#1474=LINE('',#8895,#1857);
#1475=LINE('',#8896,#1858);
#1476=LINE('',#8908,#1859);
#1477=LINE('',#8912,#1860);
#1478=LINE('',#8916,#1861);
#1479=LINE('',#8923,#1862);
#1480=LINE('',#8925,#1863);
#1481=LINE('',#10498,#1864);
#1482=LINE('',#10505,#1865);
#1483=LINE('',#10508,#1866);
#1484=LINE('',#10517,#1867);
#1485=LINE('',#10523,#1868);
#1486=LINE('',#10531,#1869);
#1487=LINE('',#10561,#1870);
#1488=LINE('',#10608,#1871);
#1489=LINE('',#10613,#1872);
#1490=LINE('',#10619,#1873);
#1491=LINE('',#10630,#1874);
#1492=LINE('',#10632,#1875);
#1493=LINE('',#10634,#1876);
#1494=LINE('',#10635,#1877);
#1495=LINE('',#10638,#1878);
#1496=LINE('',#10640,#1879);
#1497=LINE('',#10641,#1880);
#1498=LINE('',#10644,#1881);
#1499=LINE('',#10646,#1882);
#1500=LINE('',#10647,#1883);
#1501=LINE('',#10650,#1884);
#1502=LINE('',#10652,#1885);
#1503=LINE('',#10653,#1886);
#1504=LINE('',#10656,#1887);
#1505=LINE('',#10658,#1888);
#1506=LINE('',#10659,#1889);
#1507=LINE('',#10661,#1890);
#1508=LINE('',#10662,#1891);
#1509=LINE('',#10670,#1892);
#1510=LINE('',#10672,#1893);
#1511=LINE('',#10677,#1894);
#1512=LINE('',#10698,#1895);
#1513=LINE('',#10753,#1896);
#1514=LINE('',#10758,#1897);
#1515=LINE('',#10766,#1898);
#1516=LINE('',#10770,#1899);
#1517=LINE('',#10772,#1900);
#1518=LINE('',#10774,#1901);
#1519=LINE('',#10775,#1902);
#1520=LINE('',#10778,#1903);
#1521=LINE('',#10780,#1904);
#1522=LINE('',#10781,#1905);
#1523=LINE('',#10784,#1906);
#1524=LINE('',#10786,#1907);
#1525=LINE('',#10787,#1908);
#1526=LINE('',#10790,#1909);
#1527=LINE('',#10792,#1910);
#1528=LINE('',#10793,#1911);
#1529=LINE('',#10796,#1912);
#1530=LINE('',#10798,#1913);
#1531=LINE('',#10799,#1914);
#1532=LINE('',#10802,#1915);
#1533=LINE('',#10804,#1916);
#1534=LINE('',#10805,#1917);
#1535=LINE('',#10808,#1918);
#1536=LINE('',#10810,#1919);
#1537=LINE('',#10811,#1920);
#1538=LINE('',#10814,#1921);
#1539=LINE('',#10816,#1922);
#1540=LINE('',#10817,#1923);
#1541=LINE('',#10820,#1924);
#1542=LINE('',#10822,#1925);
#1543=LINE('',#10823,#1926);
#1544=LINE('',#10826,#1927);
#1545=LINE('',#10828,#1928);
#1546=LINE('',#10829,#1929);
#1547=LINE('',#10832,#1930);
#1548=LINE('',#10834,#1931);
#1549=LINE('',#10835,#1932);
#1550=LINE('',#10838,#1933);
#1551=LINE('',#10840,#1934);
#1552=LINE('',#10841,#1935);
#1553=LINE('',#10844,#1936);
#1554=LINE('',#10846,#1937);
#1555=LINE('',#10847,#1938);
#1556=LINE('',#10850,#1939);
#1557=LINE('',#10852,#1940);
#1558=LINE('',#10853,#1941);
#1559=LINE('',#10856,#1942);
#1560=LINE('',#10858,#1943);
#1561=LINE('',#10859,#1944);
#1562=LINE('',#10862,#1945);
#1563=LINE('',#10864,#1946);
#1564=LINE('',#10865,#1947);
#1565=LINE('',#10868,#1948);
#1566=LINE('',#10870,#1949);
#1567=LINE('',#10871,#1950);
#1568=LINE('',#10874,#1951);
#1569=LINE('',#10876,#1952);
#1570=LINE('',#10877,#1953);
#1571=LINE('',#10880,#1954);
#1572=LINE('',#10882,#1955);
#1573=LINE('',#10883,#1956);
#1574=LINE('',#10886,#1957);
#1575=LINE('',#10888,#1958);
#1576=LINE('',#10889,#1959);
#1577=LINE('',#10892,#1960);
#1578=LINE('',#10894,#1961);
#1579=LINE('',#10895,#1962);
#1580=LINE('',#10898,#1963);
#1581=LINE('',#10900,#1964);
#1582=LINE('',#10901,#1965);
#1583=LINE('',#10904,#1966);
#1584=LINE('',#10906,#1967);
#1585=LINE('',#10907,#1968);
#1586=LINE('',#10910,#1969);
#1587=LINE('',#10912,#1970);
#1588=LINE('',#10913,#1971);
#1589=LINE('',#10916,#1972);
#1590=LINE('',#10918,#1973);
#1591=LINE('',#10919,#1974);
#1592=LINE('',#10922,#1975);
#1593=LINE('',#10924,#1976);
#1594=LINE('',#10925,#1977);
#1595=LINE('',#10928,#1978);
#1596=LINE('',#10930,#1979);
#1597=LINE('',#10931,#1980);
#1598=LINE('',#10934,#1981);
#1599=LINE('',#10936,#1982);
#1600=LINE('',#10937,#1983);
#1601=LINE('',#10940,#1984);
#1602=LINE('',#10942,#1985);
#1603=LINE('',#10943,#1986);
#1604=LINE('',#10946,#1987);
#1605=LINE('',#10948,#1988);
#1606=LINE('',#10949,#1989);
#1607=LINE('',#10952,#1990);
#1608=LINE('',#10954,#1991);
#1609=LINE('',#10955,#1992);
#1610=LINE('',#10958,#1993);
#1611=LINE('',#10960,#1994);
#1612=LINE('',#10961,#1995);
#1613=LINE('',#10964,#1996);
#1614=LINE('',#10966,#1997);
#1615=LINE('',#10967,#1998);
#1616=LINE('',#10970,#1999);
#1617=LINE('',#10972,#2000);
#1618=LINE('',#10973,#2001);
#1619=LINE('',#10976,#2002);
#1620=LINE('',#10978,#2003);
#1621=LINE('',#10979,#2004);
#1622=LINE('',#10982,#2005);
#1623=LINE('',#10984,#2006);
#1624=LINE('',#10985,#2007);
#1625=LINE('',#10988,#2008);
#1626=LINE('',#10990,#2009);
#1627=LINE('',#10991,#2010);
#1628=LINE('',#10994,#2011);
#1629=LINE('',#10996,#2012);
#1630=LINE('',#10997,#2013);
#1631=LINE('',#11000,#2014);
#1632=LINE('',#11002,#2015);
#1633=LINE('',#11003,#2016);
#1634=LINE('',#11006,#2017);
#1635=LINE('',#11008,#2018);
#1636=LINE('',#11009,#2019);
#1637=LINE('',#11012,#2020);
#1638=LINE('',#11014,#2021);
#1639=LINE('',#11015,#2022);
#1640=LINE('',#11018,#2023);
#1641=LINE('',#11020,#2024);
#1642=LINE('',#11021,#2025);
#1643=LINE('',#11024,#2026);
#1644=LINE('',#11026,#2027);
#1645=LINE('',#11027,#2028);
#1646=LINE('',#11030,#2029);
#1647=LINE('',#11032,#2030);
#1648=LINE('',#11033,#2031);
#1649=LINE('',#11036,#2032);
#1650=LINE('',#11038,#2033);
#1651=LINE('',#11039,#2034);
#1652=LINE('',#11042,#2035);
#1653=LINE('',#11044,#2036);
#1654=LINE('',#11045,#2037);
#1655=LINE('',#11048,#2038);
#1656=LINE('',#11050,#2039);
#1657=LINE('',#11051,#2040);
#1658=LINE('',#11053,#2041);
#1659=LINE('',#11054,#2042);
#1660=LINE('',#11061,#2043);
#1661=LINE('',#11063,#2044);
#1662=LINE('',#11065,#2045);
#1663=LINE('',#11066,#2046);
#1664=LINE('',#11069,#2047);
#1665=LINE('',#11071,#2048);
#1666=LINE('',#11072,#2049);
#1667=LINE('',#11075,#2050);
#1668=LINE('',#11077,#2051);
#1669=LINE('',#11078,#2052);
#1670=LINE('',#11081,#2053);
#1671=LINE('',#11083,#2054);
#1672=LINE('',#11084,#2055);
#1673=LINE('',#11087,#2056);
#1674=LINE('',#11089,#2057);
#1675=LINE('',#11090,#2058);
#1676=LINE('',#11092,#2059);
#1677=LINE('',#11093,#2060);
#1678=LINE('',#11101,#2061);
#1679=LINE('',#11105,#2062);
#1680=LINE('',#11109,#2063);
#1681=LINE('',#11122,#2064);
#1682=LINE('',#11126,#2065);
#1683=LINE('',#11130,#2066);
#1684=LINE('',#11132,#2067);
#1685=LINE('',#11134,#2068);
#1686=LINE('',#11136,#2069);
#1687=LINE('',#11139,#2070);
#1688=LINE('',#11146,#2071);
#1689=LINE('',#11152,#2072);
#1690=LINE('',#11156,#2073);
#1691=LINE('',#11158,#2074);
#1692=LINE('',#11160,#2075);
#1693=LINE('',#11161,#2076);
#1694=LINE('',#11164,#2077);
#1695=LINE('',#11165,#2078);
#1696=LINE('',#11167,#2079);
#1697=LINE('',#11168,#2080);
#1698=LINE('',#11170,#2081);
#1699=LINE('',#11172,#2082);
#1700=LINE('',#11177,#2083);
#1701=LINE('',#11180,#2084);
#1702=LINE('',#11183,#2085);
#1703=LINE('',#11186,#2086);
#1704=LINE('',#11187,#2087);
#1705=LINE('',#11190,#2088);
#1706=LINE('',#11191,#2089);
#1707=LINE('',#11193,#2090);
#1708=VECTOR('',#6076,0.225);
#1709=VECTOR('',#6083,0.210000000000001);
#1710=VECTOR('',#6090,0.21);
#1711=VECTOR('',#6097,0.21);
#1712=VECTOR('',#6104,0.21);
#1713=VECTOR('',#6111,0.21);
#1714=VECTOR('',#6118,0.21);
#1715=VECTOR('',#6123,1.);
#1716=VECTOR('',#6124,1.);
#1717=VECTOR('',#6125,1.);
#1718=VECTOR('',#6126,1.);
#1719=VECTOR('',#6129,1.);
#1720=VECTOR('',#6130,1.);
#1721=VECTOR('',#6131,1.);
#1722=VECTOR('',#6134,1.);
#1723=VECTOR('',#6135,1.);
#1724=VECTOR('',#6136,1.);
#1725=VECTOR('',#6139,1.);
#1726=VECTOR('',#6140,1.);
#1727=VECTOR('',#6151,0.275);
#1728=VECTOR('',#6158,0.275);
#1729=VECTOR('',#6165,0.525);
#1730=VECTOR('',#6174,0.305);
#1731=VECTOR('',#6181,0.9);
#1732=VECTOR('',#6188,1.);
#1733=VECTOR('',#6189,1.);
#1734=VECTOR('',#6190,1.);
#1735=VECTOR('',#6191,1.);
#1736=VECTOR('',#6194,1.);
#1737=VECTOR('',#6195,1.);
#1738=VECTOR('',#6196,1.);
#1739=VECTOR('',#6199,1.);
#1740=VECTOR('',#6200,1.);
#1741=VECTOR('',#6201,1.);
#1742=VECTOR('',#6204,1.);
#1743=VECTOR('',#6205,1.);
#1744=VECTOR('',#6216,0.165);
#1745=VECTOR('',#6229,0.5);
#1746=VECTOR('',#6238,0.3);
#1747=VECTOR('',#6247,0.31);
#1748=VECTOR('',#6254,0.5);
#1749=VECTOR('',#6267,0.31);
#1750=VECTOR('',#6274,0.5);
#1751=VECTOR('',#6287,0.225);
#1752=VECTOR('',#6294,0.7);
#1753=VECTOR('',#6307,0.164999999999999);
#1754=VECTOR('',#6316,0.0999999999999996);
#1755=VECTOR('',#6325,1.);
#1756=VECTOR('',#6326,1.);
#1757=VECTOR('',#6327,1.);
#1758=VECTOR('',#6328,1.);
#1759=VECTOR('',#6329,1.);
#1760=VECTOR('',#6332,1.);
#1761=VECTOR('',#6333,1.);
#1762=VECTOR('',#6334,1.);
#1763=VECTOR('',#6339,1.);
#1764=VECTOR('',#6340,1.);
#1765=VECTOR('',#6343,1.);
#1766=VECTOR('',#6344,1.);
#1767=VECTOR('',#6347,1.);
#1768=VECTOR('',#6350,1.);
#1769=VECTOR('',#6355,0.300000000000001);
#1770=VECTOR('',#6364,0.25);
#1771=VECTOR('',#6369,0.165);
#1772=VECTOR('',#6378,0.165);
#1773=VECTOR('',#6387,0.165);
#1774=VECTOR('',#6396,0.165);
#1775=VECTOR('',#6409,1.);
#1776=VECTOR('',#6412,1.);
#1777=VECTOR('',#6415,1.);
#1778=VECTOR('',#6418,1.);
#1779=VECTOR('',#6427,1.);
#1780=VECTOR('',#6430,1.);
#1781=VECTOR('',#6439,1.);
#1782=VECTOR('',#6442,1.);
#1783=VECTOR('',#6453,2.2);
#1784=VECTOR('',#6480,0.275);
#1785=VECTOR('',#6485,0.275);
#1786=VECTOR('',#6490,0.275);
#1787=VECTOR('',#6495,0.275);
#1788=VECTOR('',#6500,1.5);
#1789=VECTOR('',#6509,3.);
#1790=VECTOR('',#6514,1.02);
#1791=VECTOR('',#6527,0.375);
#1792=VECTOR('',#6538,0.375);
#1793=VECTOR('',#6549,0.375);
#1794=VECTOR('',#6560,0.375);
#1795=VECTOR('',#6571,0.225);
#1796=VECTOR('',#6576,0.225);
#1797=VECTOR('',#6581,0.225);
#1798=VECTOR('',#6586,0.225);
#1799=VECTOR('',#6591,1.49);
#1800=VECTOR('',#6602,0.71);
#1801=VECTOR('',#6607,2.2);
#1802=VECTOR('',#6632,0.976185);
#1803=VECTOR('',#6639,0.5);
#1804=VECTOR('',#6644,0.53);
#1805=VECTOR('',#6653,0.976185);
#1806=VECTOR('',#6660,0.53);
#1807=VECTOR('',#6679,1.023815);
#1808=VECTOR('',#6690,1.47);
#1809=VECTOR('',#6695,1.5);
#1810=VECTOR('',#6700,1.47);
#1811=VECTOR('',#6705,1.023815);
#1812=VECTOR('',#6756,1.019052);
#1813=VECTOR('',#6833,0.980948);
#1814=VECTOR('',#6862,1.013815);
#1815=VECTOR('',#6869,0.991185);
#1816=VECTOR('',#6880,1.013815);
#1817=VECTOR('',#6887,0.991185);
#1818=VECTOR('',#6902,1.);
#1819=VECTOR('',#6903,1.);
#1820=VECTOR('',#6904,1.);
#1821=VECTOR('',#6905,1.);
#1822=VECTOR('',#6908,1.);
#1823=VECTOR('',#6909,1.);
#1824=VECTOR('',#6910,1.);
#1825=VECTOR('',#6913,1.);
#1826=VECTOR('',#6914,1.);
#1827=VECTOR('',#6915,1.);
#1828=VECTOR('',#6918,1.);
#1829=VECTOR('',#6919,1.);
#1830=VECTOR('',#6920,1.);
#1831=VECTOR('',#6923,1.);
#1832=VECTOR('',#6924,1.);
#1833=VECTOR('',#6925,1.);
#1834=VECTOR('',#6928,1.);
#1835=VECTOR('',#6929,1.);
#1836=VECTOR('',#6946,0.4);
#1837=VECTOR('',#6951,0.425);
#1838=VECTOR('',#6956,0.41);
#1839=VECTOR('',#6965,0.26);
#1840=VECTOR('',#6968,0.25);
#1841=VECTOR('',#6973,1.);
#1842=VECTOR('',#6974,1.);
#1843=VECTOR('',#6975,1.);
#1844=VECTOR('',#6976,1.);
#1845=VECTOR('',#6979,1.);
#1846=VECTOR('',#6980,1.);
#1847=VECTOR('',#6981,1.);
#1848=VECTOR('',#6984,1.);
#1849=VECTOR('',#6985,1.);
#1850=VECTOR('',#6986,1.);
#1851=VECTOR('',#6989,1.);
#1852=VECTOR('',#6990,1.);
#1853=VECTOR('',#6991,1.);
#1854=VECTOR('',#6994,1.);
#1855=VECTOR('',#6995,1.);
#1856=VECTOR('',#6996,1.);
#1857=VECTOR('',#6999,1.);
#1858=VECTOR('',#7000,1.);
#1859=VECTOR('',#7017,0.325);
#1860=VECTOR('',#7022,0.35);
#1861=VECTOR('',#7027,0.335);
#1862=VECTOR('',#7036,0.21);
#1863=VECTOR('',#7039,0.2);
#1864=VECTOR('',#7118,1.);
#1865=VECTOR('',#7127,0.7);
#1866=VECTOR('',#7130,0.5);
#1867=VECTOR('',#7143,0.505);
#1868=VECTOR('',#7150,0.7);
#1869=VECTOR('',#7161,1.);
#1870=VECTOR('',#7168,0.165);
#1871=VECTOR('',#7171,1.);
#1872=VECTOR('',#7176,0.505);
#1873=VECTOR('',#7183,0.9);
#1874=VECTOR('',#7198,1.);
#1875=VECTOR('',#7199,1.);
#1876=VECTOR('',#7200,1.);
#1877=VECTOR('',#7201,1.);
#1878=VECTOR('',#7204,1.);
#1879=VECTOR('',#7205,1.);
#1880=VECTOR('',#7206,1.);
#1881=VECTOR('',#7209,1.);
#1882=VECTOR('',#7210,1.);
#1883=VECTOR('',#7211,1.);
#1884=VECTOR('',#7214,1.);
#1885=VECTOR('',#7215,1.);
#1886=VECTOR('',#7216,1.);
#1887=VECTOR('',#7219,1.);
#1888=VECTOR('',#7220,1.);
#1889=VECTOR('',#7221,1.);
#1890=VECTOR('',#7224,1.);
#1891=VECTOR('',#7225,1.);
#1892=VECTOR('',#7236,0.185);
#1893=VECTOR('',#7239,0.2);
#1894=VECTOR('',#7244,1.);
#1895=VECTOR('',#7251,0.21);
#1896=VECTOR('',#7256,1.);
#1897=VECTOR('',#7261,1.6);
#1898=VECTOR('',#7272,1.005);
#1899=VECTOR('',#7275,1.);
#1900=VECTOR('',#7276,1.);
#1901=VECTOR('',#7277,1.);
#1902=VECTOR('',#7278,1.);
#1903=VECTOR('',#7281,1.);
#1904=VECTOR('',#7282,1.);
#1905=VECTOR('',#7283,1.);
#1906=VECTOR('',#7286,1.);
#1907=VECTOR('',#7287,1.);
#1908=VECTOR('',#7288,1.);
#1909=VECTOR('',#7291,1.);
#1910=VECTOR('',#7292,1.);
#1911=VECTOR('',#7293,1.);
#1912=VECTOR('',#7296,1.);
#1913=VECTOR('',#7297,1.);
#1914=VECTOR('',#7298,1.);
#1915=VECTOR('',#7301,1.);
#1916=VECTOR('',#7302,1.);
#1917=VECTOR('',#7303,1.);
#1918=VECTOR('',#7306,1.);
#1919=VECTOR('',#7307,1.);
#1920=VECTOR('',#7308,1.);
#1921=VECTOR('',#7311,1.);
#1922=VECTOR('',#7312,1.);
#1923=VECTOR('',#7313,1.);
#1924=VECTOR('',#7316,1.);
#1925=VECTOR('',#7317,1.);
#1926=VECTOR('',#7318,1.);
#1927=VECTOR('',#7321,1.);
#1928=VECTOR('',#7322,1.);
#1929=VECTOR('',#7323,1.);
#1930=VECTOR('',#7326,1.);
#1931=VECTOR('',#7327,1.);
#1932=VECTOR('',#7328,1.);
#1933=VECTOR('',#7331,1.);
#1934=VECTOR('',#7332,1.);
#1935=VECTOR('',#7333,1.);
#1936=VECTOR('',#7336,1.);
#1937=VECTOR('',#7337,1.);
#1938=VECTOR('',#7338,1.);
#1939=VECTOR('',#7341,1.);
#1940=VECTOR('',#7342,1.);
#1941=VECTOR('',#7343,1.);
#1942=VECTOR('',#7346,1.);
#1943=VECTOR('',#7347,1.);
#1944=VECTOR('',#7348,1.);
#1945=VECTOR('',#7351,1.);
#1946=VECTOR('',#7352,1.);
#1947=VECTOR('',#7353,1.);
#1948=VECTOR('',#7356,1.);
#1949=VECTOR('',#7357,1.);
#1950=VECTOR('',#7358,1.);
#1951=VECTOR('',#7361,1.);
#1952=VECTOR('',#7362,1.);
#1953=VECTOR('',#7363,1.);
#1954=VECTOR('',#7366,1.);
#1955=VECTOR('',#7367,1.);
#1956=VECTOR('',#7368,1.);
#1957=VECTOR('',#7371,1.);
#1958=VECTOR('',#7372,1.);
#1959=VECTOR('',#7373,1.);
#1960=VECTOR('',#7376,1.);
#1961=VECTOR('',#7377,1.);
#1962=VECTOR('',#7378,1.);
#1963=VECTOR('',#7381,1.);
#1964=VECTOR('',#7382,1.);
#1965=VECTOR('',#7383,1.);
#1966=VECTOR('',#7386,1.);
#1967=VECTOR('',#7387,1.);
#1968=VECTOR('',#7388,1.);
#1969=VECTOR('',#7391,1.);
#1970=VECTOR('',#7392,1.);
#1971=VECTOR('',#7393,1.);
#1972=VECTOR('',#7396,1.);
#1973=VECTOR('',#7397,1.);
#1974=VECTOR('',#7398,1.);
#1975=VECTOR('',#7401,1.);
#1976=VECTOR('',#7402,1.);
#1977=VECTOR('',#7403,1.);
#1978=VECTOR('',#7406,1.);
#1979=VECTOR('',#7407,1.);
#1980=VECTOR('',#7408,1.);
#1981=VECTOR('',#7411,1.);
#1982=VECTOR('',#7412,1.);
#1983=VECTOR('',#7413,1.);
#1984=VECTOR('',#7416,1.);
#1985=VECTOR('',#7417,1.);
#1986=VECTOR('',#7418,1.);
#1987=VECTOR('',#7421,1.);
#1988=VECTOR('',#7422,1.);
#1989=VECTOR('',#7423,1.);
#1990=VECTOR('',#7426,1.);
#1991=VECTOR('',#7427,1.);
#1992=VECTOR('',#7428,1.);
#1993=VECTOR('',#7431,1.);
#1994=VECTOR('',#7432,1.);
#1995=VECTOR('',#7433,1.);
#1996=VECTOR('',#7436,1.);
#1997=VECTOR('',#7437,1.);
#1998=VECTOR('',#7438,1.);
#1999=VECTOR('',#7441,1.);
#2000=VECTOR('',#7442,1.);
#2001=VECTOR('',#7443,1.);
#2002=VECTOR('',#7446,1.);
#2003=VECTOR('',#7447,1.);
#2004=VECTOR('',#7448,1.);
#2005=VECTOR('',#7451,1.);
#2006=VECTOR('',#7452,1.);
#2007=VECTOR('',#7453,1.);
#2008=VECTOR('',#7456,1.);
#2009=VECTOR('',#7457,1.);
#2010=VECTOR('',#7458,1.);
#2011=VECTOR('',#7461,1.);
#2012=VECTOR('',#7462,1.);
#2013=VECTOR('',#7463,1.);
#2014=VECTOR('',#7466,1.);
#2015=VECTOR('',#7467,1.);
#2016=VECTOR('',#7468,1.);
#2017=VECTOR('',#7471,1.);
#2018=VECTOR('',#7472,1.);
#2019=VECTOR('',#7473,1.);
#2020=VECTOR('',#7476,1.);
#2021=VECTOR('',#7477,1.);
#2022=VECTOR('',#7478,1.);
#2023=VECTOR('',#7481,1.);
#2024=VECTOR('',#7482,1.);
#2025=VECTOR('',#7483,1.);
#2026=VECTOR('',#7486,1.);
#2027=VECTOR('',#7487,1.);
#2028=VECTOR('',#7488,1.);
#2029=VECTOR('',#7491,1.);
#2030=VECTOR('',#7492,1.);
#2031=VECTOR('',#7493,1.);
#2032=VECTOR('',#7496,1.);
#2033=VECTOR('',#7497,1.);
#2034=VECTOR('',#7498,1.);
#2035=VECTOR('',#7501,1.);
#2036=VECTOR('',#7502,1.);
#2037=VECTOR('',#7503,1.);
#2038=VECTOR('',#7506,1.);
#2039=VECTOR('',#7507,1.);
#2040=VECTOR('',#7508,1.);
#2041=VECTOR('',#7511,1.);
#2042=VECTOR('',#7512,1.);
#2043=VECTOR('',#7521,1.);
#2044=VECTOR('',#7522,1.);
#2045=VECTOR('',#7523,1.);
#2046=VECTOR('',#7524,1.);
#2047=VECTOR('',#7527,1.);
#2048=VECTOR('',#7528,1.);
#2049=VECTOR('',#7529,1.);
#2050=VECTOR('',#7532,1.);
#2051=VECTOR('',#7533,1.);
#2052=VECTOR('',#7534,1.);
#2053=VECTOR('',#7537,1.);
#2054=VECTOR('',#7538,1.);
#2055=VECTOR('',#7539,1.);
#2056=VECTOR('',#7542,1.);
#2057=VECTOR('',#7543,1.);
#2058=VECTOR('',#7544,1.);
#2059=VECTOR('',#7547,1.);
#2060=VECTOR('',#7548,1.);
#2061=VECTOR('',#7559,0.235);
#2062=VECTOR('',#7564,0.25);
#2063=VECTOR('',#7569,0.2125);
#2064=VECTOR('',#7590,1.);
#2065=VECTOR('',#7593,1.);
#2066=VECTOR('',#7598,1.);
#2067=VECTOR('',#7599,1.);
#2068=VECTOR('',#7600,1.);
#2069=VECTOR('',#7601,1.);
#2070=VECTOR('',#7604,1.);
#2071=VECTOR('',#7611,0.0999999999999996);
#2072=VECTOR('',#7620,1.);
#2073=VECTOR('',#7625,1.);
#2074=VECTOR('',#7626,1.);
#2075=VECTOR('',#7627,1.);
#2076=VECTOR('',#7628,1.);
#2077=VECTOR('',#7631,1.);
#2078=VECTOR('',#7632,1.);
#2079=VECTOR('',#7633,1.);
#2080=VECTOR('',#7634,1.);
#2081=VECTOR('',#7637,1.);
#2082=VECTOR('',#7640,1.);
#2083=VECTOR('',#7647,0.305);
#2084=VECTOR('',#7650,1.);
#2085=VECTOR('',#7653,1.);
#2086=VECTOR('',#7656,1.);
#2087=VECTOR('',#7657,1.);
#2088=VECTOR('',#7660,1.);
#2089=VECTOR('',#7661,1.);
#2090=VECTOR('',#7664,1.);
#2091=CIRCLE('',#5457,0.225);
#2092=CIRCLE('',#5458,0.225);
#2093=CIRCLE('',#5460,0.210000000000001);
#2094=CIRCLE('',#5461,0.210000000000001);
#2095=CIRCLE('',#5463,0.21);
#2096=CIRCLE('',#5464,0.21);
#2097=CIRCLE('',#5466,0.21);
#2098=CIRCLE('',#5467,0.21);
#2099=CIRCLE('',#5469,0.21);
#2100=CIRCLE('',#5470,0.21);
#2101=CIRCLE('',#5472,0.21);
#2102=CIRCLE('',#5473,0.21);
#2103=CIRCLE('',#5475,0.21);
#2104=CIRCLE('',#5476,0.21);
#2105=CIRCLE('',#5485,0.275);
#2106=CIRCLE('',#5486,0.275);
#2107=CIRCLE('',#5488,0.275);
#2108=CIRCLE('',#5489,0.275);
#2109=CIRCLE('',#5491,0.525);
#2110=CIRCLE('',#5492,0.525);
#2111=CIRCLE('',#5494,0.305);
#2112=CIRCLE('',#5496,0.305);
#2113=CIRCLE('',#5498,0.9);
#2114=CIRCLE('',#5499,0.9);
#2115=CIRCLE('',#5509,0.165);
#2116=CIRCLE('',#5510,0.165);
#2117=CIRCLE('',#5513,0.5);
#2118=CIRCLE('',#5514,0.3);
#2119=CIRCLE('',#5516,0.5);
#2120=CIRCLE('',#5519,0.3);
#2121=CIRCLE('',#5523,0.31);
#2122=CIRCLE('',#5524,0.31);
#2123=CIRCLE('',#5526,0.5);
#2124=CIRCLE('',#5527,0.5);
#2125=CIRCLE('',#5532,0.31);
#2126=CIRCLE('',#5533,0.31);
#2127=CIRCLE('',#5535,0.5);
#2128=CIRCLE('',#5536,0.5);
#2129=CIRCLE('',#5541,0.225);
#2130=CIRCLE('',#5542,0.225);
#2131=CIRCLE('',#5544,0.7);
#2132=CIRCLE('',#5545,0.7);
#2133=CIRCLE('',#5550,0.164999999999999);
#2134=CIRCLE('',#5551,0.164999999999999);
#2135=CIRCLE('',#5554,0.0999999999999996);
#2136=CIRCLE('',#5555,0.0999999999999996);
#2137=CIRCLE('',#5556,0.0999999999999996);
#2138=CIRCLE('',#5560,0.300000000000001);
#2139=CIRCLE('',#5561,0.300000000000001);
#2140=CIRCLE('',#5567,0.300000000000001);
#2141=CIRCLE('',#5572,0.165);
#2142=CIRCLE('',#5573,0.165);
#2143=CIRCLE('',#5576,0.165);
#2144=CIRCLE('',#5577,0.165);
#2145=CIRCLE('',#5580,0.165);
#2146=CIRCLE('',#5581,0.165);
#2147=CIRCLE('',#5584,0.165);
#2148=CIRCLE('',#5585,0.165);
#2149=CIRCLE('',#5588,2.2);
#2150=CIRCLE('',#5589,0.525);
#2151=CIRCLE('',#5591,0.525);
#2152=CIRCLE('',#5593,0.525);
#2153=CIRCLE('',#5594,0.525);
#2154=CIRCLE('',#5596,2.2);
#2155=CIRCLE('',#5598,0.525);
#2156=CIRCLE('',#5599,0.525);
#2157=CIRCLE('',#5601,2.2);
#2158=CIRCLE('',#5603,0.525);
#2159=CIRCLE('',#5604,0.525);
#2160=CIRCLE('',#5606,2.2);
#2161=CIRCLE('',#5608,2.2);
#2162=CIRCLE('',#5609,2.2);
#2163=CIRCLE('',#5610,2.2);
#2164=CIRCLE('',#5611,2.2);
#2165=CIRCLE('',#5612,2.2);
#2166=CIRCLE('',#5613,2.2);
#2167=CIRCLE('',#5615,3.);
#2168=CIRCLE('',#5616,0.275);
#2169=CIRCLE('',#5617,0.275);
#2170=CIRCLE('',#5618,0.275);
#2171=CIRCLE('',#5619,0.275);
#2172=CIRCLE('',#5621,0.275);
#2173=CIRCLE('',#5623,0.275);
#2174=CIRCLE('',#5625,0.275);
#2175=CIRCLE('',#5627,0.275);
#2176=CIRCLE('',#5629,1.5);
#2177=CIRCLE('',#5630,1.5);
#2178=CIRCLE('',#5632,1.02);
#2179=CIRCLE('',#5634,3.);
#2180=CIRCLE('',#5636,1.02);
#2181=CIRCLE('',#5641,0.375);
#2182=CIRCLE('',#5642,0.375);
#2183=CIRCLE('',#5644,0.225);
#2184=CIRCLE('',#5646,0.375);
#2185=CIRCLE('',#5647,0.375);
#2186=CIRCLE('',#5649,0.225);
#2187=CIRCLE('',#5651,0.375);
#2188=CIRCLE('',#5652,0.375);
#2189=CIRCLE('',#5654,0.225);
#2190=CIRCLE('',#5656,0.375);
#2191=CIRCLE('',#5657,0.375);
#2192=CIRCLE('',#5659,0.225);
#2193=CIRCLE('',#5661,0.225);
#2194=CIRCLE('',#5663,0.225);
#2195=CIRCLE('',#5665,0.225);
#2196=CIRCLE('',#5667,0.225);
#2197=CIRCLE('',#5669,1.49);
#2198=CIRCLE('',#5670,1.49);
#2199=CIRCLE('',#5672,0.71);
#2200=CIRCLE('',#5674,0.71);
#2201=CIRCLE('',#5676,2.2);
#2202=CIRCLE('',#5677,2.2);
#2203=CIRCLE('',#5683,0.976185);
#2204=CIRCLE('',#5684,0.976185);
#2205=CIRCLE('',#5685,0.247676);
#2206=CIRCLE('',#5686,0.976185);
#2207=CIRCLE('',#5687,0.976185);
#2208=CIRCLE('',#5689,0.976185);
#2209=CIRCLE('',#5691,0.5);
#2210=CIRCLE('',#5692,0.5);
#2211=CIRCLE('',#5694,0.56);
#2212=CIRCLE('',#5697,0.976185);
#2213=CIRCLE('',#5699,0.56);
#2214=CIRCLE('',#5703,1.023815);
#2215=CIRCLE('',#5704,1.023815);
#2216=CIRCLE('',#5705,0.247676);
#2217=CIRCLE('',#5706,1.023815);
#2218=CIRCLE('',#5707,1.023815);
#2219=CIRCLE('',#5709,1.023815);
#2220=CIRCLE('',#5711,1.44);
#2221=CIRCLE('',#5712,1.023815);
#2222=CIRCLE('',#5714,1.5);
#2223=CIRCLE('',#5716,1.5);
#2224=CIRCLE('',#5718,1.44);
#2225=CIRCLE('',#5723,0.23815);
#2226=CIRCLE('',#5725,0.23815);
#2227=CIRCLE('',#5727,0.23815);
#2228=CIRCLE('',#5729,0.23815);
#2229=CIRCLE('',#5731,0.23815);
#2230=CIRCLE('',#5733,0.23815);
#2231=CIRCLE('',#5735,0.23815);
#2232=CIRCLE('',#5737,0.23815);
#2233=CIRCLE('',#5740,0.243053047864041);
#2234=CIRCLE('',#5741,0.243053047864041);
#2235=CIRCLE('',#5743,1.019052);
#2236=CIRCLE('',#5744,1.019052);
#2237=CIRCLE('',#5745,1.019052);
#2238=CIRCLE('',#5746,1.019052);
#2239=CIRCLE('',#5747,1.019052);
#2240=CIRCLE('',#5748,1.019052);
#2241=CIRCLE('',#5749,1.019052);
#2242=CIRCLE('',#5750,1.019052);
#2243=CIRCLE('',#5751,1.019052);
#2244=CIRCLE('',#5753,0.980948);
#2245=CIRCLE('',#5754,0.243053047864041);
#2246=CIRCLE('',#5756,0.243053047864041);
#2247=CIRCLE('',#5758,0.980948);
#2248=CIRCLE('',#5759,0.243053047864041);
#2249=CIRCLE('',#5761,0.243053047864041);
#2250=CIRCLE('',#5763,0.980948);
#2251=CIRCLE('',#5764,0.243053047864041);
#2252=CIRCLE('',#5766,0.243053047864041);
#2253=CIRCLE('',#5768,0.980948);
#2254=CIRCLE('',#5769,0.243053047864041);
#2255=CIRCLE('',#5771,0.243053047864041);
#2256=CIRCLE('',#5773,0.980948);
#2257=CIRCLE('',#5774,0.243053047864041);
#2258=CIRCLE('',#5776,0.243053047864041);
#2259=CIRCLE('',#5778,0.980948);
#2260=CIRCLE('',#5779,0.243053047864041);
#2261=CIRCLE('',#5781,0.243053047864041);
#2262=CIRCLE('',#5783,0.980948);
#2263=CIRCLE('',#5784,0.980948);
#2264=CIRCLE('',#5785,0.980948);
#2265=CIRCLE('',#5787,0.243053047864041);
#2266=CIRCLE('',#5789,0.243053047864041);
#2267=CIRCLE('',#5794,1.013815);
#2268=CIRCLE('',#5795,0.991185);
#2269=CIRCLE('',#5797,1.013815);
#2270=CIRCLE('',#5799,0.991185);
#2271=CIRCLE('',#5802,1.013815);
#2272=CIRCLE('',#5803,0.991185);
#2273=CIRCLE('',#5805,1.013815);
#2274=CIRCLE('',#5807,0.991185);
#2275=CIRCLE('',#5824,0.24505);
#2276=CIRCLE('',#5826,0.375);
#2277=CIRCLE('',#5828,0.425);
#2278=CIRCLE('',#5830,0.425);
#2279=CIRCLE('',#5832,0.395);
#2280=CIRCLE('',#5834,0.27);
#2281=CIRCLE('',#5836,0.24505);
#2282=CIRCLE('',#5848,0.1954);
#2283=CIRCLE('',#5850,0.3);
#2284=CIRCLE('',#5852,0.35);
#2285=CIRCLE('',#5854,0.35);
#2286=CIRCLE('',#5856,0.32);
#2287=CIRCLE('',#5858,0.22);
#2288=CIRCLE('',#5860,0.1954);
#2289=CIRCLE('',#5863,0.08);
#2290=CIRCLE('',#5864,0.08);
#2291=CIRCLE('',#5865,0.08);
#2292=CIRCLE('',#5866,0.08);
#2293=CIRCLE('',#5867,0.08);
#2294=CIRCLE('',#5868,0.08);
#2295=CIRCLE('',#5897,1.);
#2296=CIRCLE('',#5898,0.7);
#2297=CIRCLE('',#5900,1.);
#2298=CIRCLE('',#5902,0.7);
#2299=CIRCLE('',#5903,0.5);
#2300=CIRCLE('',#5906,0.5);
#2301=CIRCLE('',#5911,0.505);
#2302=CIRCLE('',#5912,0.505);
#2303=CIRCLE('',#5914,0.7);
#2304=CIRCLE('',#5915,0.7);
#2305=CIRCLE('',#5920,0.165);
#2306=CIRCLE('',#5922,0.165);
#2307=CIRCLE('',#5925,0.505);
#2308=CIRCLE('',#5926,0.505);
#2309=CIRCLE('',#5928,0.9);
#2310=CIRCLE('',#5929,0.9);
#2311=CIRCLE('',#5934,0.1954);
#2312=CIRCLE('',#5943,0.17);
#2313=CIRCLE('',#5945,0.1954);
#2314=CIRCLE('',#5949,0.21);
#2315=CIRCLE('',#5951,0.21);
#2316=CIRCLE('',#5952,0.21);
#2317=CIRCLE('',#5955,1.6);
#2318=CIRCLE('',#5956,1.6);
#2319=CIRCLE('',#5958,1.005);
#2320=CIRCLE('',#5960,1.005);
#2321=CIRCLE('',#6020,0.22);
#2322=CIRCLE('',#6022,0.24505);
#2323=CIRCLE('',#6024,0.24505);
#2324=CIRCLE('',#6026,0.175);
#2325=CIRCLE('',#6037,0.51);
#2326=CIRCLE('',#6038,0.51);
#2327=CIRCLE('',#6040,0.7);
#2328=CIRCLE('',#6041,0.305);
#2329=CIRCLE('',#6043,0.0999999999999996);
#2330=CIRCLE('',#6044,0.0999999999999996);
#2331=CIRCLE('',#6045,0.0999999999999996);
#2332=CIRCLE('',#6049,0.7);
#2333=CIRCLE('',#6055,0.305);
#2334=CIRCLE('',#6057,0.7);
#2335=VERTEX_POINT('',#7679);
#2336=VERTEX_POINT('',#7681);
#2337=VERTEX_POINT('',#7685);
#2338=VERTEX_POINT('',#7687);
#2339=VERTEX_POINT('',#7691);
#2340=VERTEX_POINT('',#7693);
#2341=VERTEX_POINT('',#7697);
#2342=VERTEX_POINT('',#7699);
#2343=VERTEX_POINT('',#7703);
#2344=VERTEX_POINT('',#7705);
#2345=VERTEX_POINT('',#7709);
#2346=VERTEX_POINT('',#7711);
#2347=VERTEX_POINT('',#7715);
#2348=VERTEX_POINT('',#7717);
#2349=VERTEX_POINT('',#7721);
#2350=VERTEX_POINT('',#7722);
#2351=VERTEX_POINT('',#7724);
#2352=VERTEX_POINT('',#7726);
#2353=VERTEX_POINT('',#7730);
#2354=VERTEX_POINT('',#7732);
#2355=VERTEX_POINT('',#7736);
#2356=VERTEX_POINT('',#7738);
#2357=VERTEX_POINT('',#7748);
#2358=VERTEX_POINT('',#7750);
#2359=VERTEX_POINT('',#7754);
#2360=VERTEX_POINT('',#7756);
#2361=VERTEX_POINT('',#7760);
#2362=VERTEX_POINT('',#7762);
#2363=VERTEX_POINT('',#7766);
#2364=VERTEX_POINT('',#7769);
#2365=VERTEX_POINT('',#7773);
#2366=VERTEX_POINT('',#7775);
#2367=VERTEX_POINT('',#7780);
#2368=VERTEX_POINT('',#7781);
#2369=VERTEX_POINT('',#7783);
#2370=VERTEX_POINT('',#7785);
#2371=VERTEX_POINT('',#7789);
#2372=VERTEX_POINT('',#7791);
#2373=VERTEX_POINT('',#7795);
#2374=VERTEX_POINT('',#7797);
#2375=VERTEX_POINT('',#7807);
#2376=VERTEX_POINT('',#7809);
#2377=VERTEX_POINT('',#7814);
#2378=VERTEX_POINT('',#7816);
#2379=VERTEX_POINT('',#7819);
#2380=VERTEX_POINT('',#7824);
#2381=VERTEX_POINT('',#7830);
#2382=VERTEX_POINT('',#7832);
#2383=VERTEX_POINT('',#7836);
#2384=VERTEX_POINT('',#7838);
#2385=VERTEX_POINT('',#7845);
#2386=VERTEX_POINT('',#7847);
#2387=VERTEX_POINT('',#7851);
#2388=VERTEX_POINT('',#7853);
#2389=VERTEX_POINT('',#7860);
#2390=VERTEX_POINT('',#7862);
#2391=VERTEX_POINT('',#7866);
#2392=VERTEX_POINT('',#7868);
#2393=VERTEX_POINT('',#7875);
#2394=VERTEX_POINT('',#7877);
#2395=VERTEX_POINT('',#7882);
#2396=VERTEX_POINT('',#7884);
#2397=VERTEX_POINT('',#7886);
#2398=VERTEX_POINT('',#7891);
#2399=VERTEX_POINT('',#7892);
#2400=VERTEX_POINT('',#7895);
#2401=VERTEX_POINT('',#7897);
#2402=VERTEX_POINT('',#7901);
#2403=VERTEX_POINT('',#7902);
#2404=VERTEX_POINT('',#7904);
#2405=VERTEX_POINT('',#7906);
#2406=VERTEX_POINT('',#7908);
#2407=VERTEX_POINT('',#7911);
#2408=VERTEX_POINT('',#7923);
#2409=VERTEX_POINT('',#7929);
#2410=VERTEX_POINT('',#7930);
#2411=VERTEX_POINT('',#7967);
#2412=VERTEX_POINT('',#7969);
#2413=VERTEX_POINT('',#8007);
#2414=VERTEX_POINT('',#8009);
#2415=VERTEX_POINT('',#8014);
#2416=VERTEX_POINT('',#8016);
#2417=VERTEX_POINT('',#8021);
#2418=VERTEX_POINT('',#8023);
#2419=VERTEX_POINT('',#8028);
#2420=VERTEX_POINT('',#8030);
#2421=VERTEX_POINT('',#8035);
#2422=VERTEX_POINT('',#8036);
#2423=VERTEX_POINT('',#8040);
#2424=VERTEX_POINT('',#8042);
#2425=VERTEX_POINT('',#8046);
#2426=VERTEX_POINT('',#8047);
#2427=VERTEX_POINT('',#8049);
#2428=VERTEX_POINT('',#8051);
#2429=VERTEX_POINT('',#8057);
#2430=VERTEX_POINT('',#8058);
#2431=VERTEX_POINT('',#8060);
#2432=VERTEX_POINT('',#8062);
#2433=VERTEX_POINT('',#8068);
#2434=VERTEX_POINT('',#8069);
#2435=VERTEX_POINT('',#8071);
#2436=VERTEX_POINT('',#8073);
#2437=VERTEX_POINT('',#8079);
#2438=VERTEX_POINT('',#8081);
#2439=VERTEX_POINT('',#8089);
#2440=VERTEX_POINT('',#8091);
#2441=VERTEX_POINT('',#8093);
#2442=VERTEX_POINT('',#8095);
#2443=VERTEX_POINT('',#8097);
#2444=VERTEX_POINT('',#8100);
#2445=VERTEX_POINT('',#8104);
#2446=VERTEX_POINT('',#8108);
#2447=VERTEX_POINT('',#8112);
#2448=VERTEX_POINT('',#8116);
#2449=VERTEX_POINT('',#8118);
#2450=VERTEX_POINT('',#8122);
#2451=VERTEX_POINT('',#8125);
#2452=VERTEX_POINT('',#8129);
#2453=VERTEX_POINT('',#8136);
#2454=VERTEX_POINT('',#8138);
#2455=VERTEX_POINT('',#8142);
#2456=VERTEX_POINT('',#8145);
#2457=VERTEX_POINT('',#8147);
#2458=VERTEX_POINT('',#8151);
#2459=VERTEX_POINT('',#8154);
#2460=VERTEX_POINT('',#8156);
#2461=VERTEX_POINT('',#8160);
#2462=VERTEX_POINT('',#8163);
#2463=VERTEX_POINT('',#8165);
#2464=VERTEX_POINT('',#8169);
#2465=VERTEX_POINT('',#8172);
#2466=VERTEX_POINT('',#8176);
#2467=VERTEX_POINT('',#8180);
#2468=VERTEX_POINT('',#8184);
#2469=VERTEX_POINT('',#8188);
#2470=VERTEX_POINT('',#8190);
#2471=VERTEX_POINT('',#8194);
#2472=VERTEX_POINT('',#8197);
#2473=VERTEX_POINT('',#8201);
#2474=VERTEX_POINT('',#8203);
#2475=VERTEX_POINT('',#8211);
#2476=VERTEX_POINT('',#8212);
#2477=VERTEX_POINT('',#8215);
#2478=VERTEX_POINT('',#8217);
#2479=VERTEX_POINT('',#8221);
#2480=VERTEX_POINT('',#8225);
#2481=VERTEX_POINT('',#8227);
#2482=VERTEX_POINT('',#8231);
#2483=VERTEX_POINT('',#8236);
#2484=VERTEX_POINT('',#8240);
#2485=VERTEX_POINT('',#8246);
#2486=VERTEX_POINT('',#8247);
#2487=VERTEX_POINT('',#8250);
#2488=VERTEX_POINT('',#8252);
#2489=VERTEX_POINT('',#8256);
#2490=VERTEX_POINT('',#8260);
#2491=VERTEX_POINT('',#8262);
#2492=VERTEX_POINT('',#8265);
#2493=VERTEX_POINT('',#8269);
#2494=VERTEX_POINT('',#8273);
#2495=VERTEX_POINT('',#8281);
#2496=VERTEX_POINT('',#8282);
#2497=VERTEX_POINT('',#8285);
#2498=VERTEX_POINT('',#8286);
#2499=VERTEX_POINT('',#8289);
#2500=VERTEX_POINT('',#8290);
#2501=VERTEX_POINT('',#8293);
#2502=VERTEX_POINT('',#8294);
#2503=VERTEX_POINT('',#8297);
#2504=VERTEX_POINT('',#8298);
#2505=VERTEX_POINT('',#8301);
#2506=VERTEX_POINT('',#8302);
#2507=VERTEX_POINT('',#8305);
#2508=VERTEX_POINT('',#8306);
#2509=VERTEX_POINT('',#8309);
#2510=VERTEX_POINT('',#8310);
#2511=VERTEX_POINT('',#8314);
#2512=VERTEX_POINT('',#8315);
#2513=VERTEX_POINT('',#8338);
#2514=VERTEX_POINT('',#8340);
#2515=VERTEX_POINT('',#8365);
#2516=VERTEX_POINT('',#8367);
#2517=VERTEX_POINT('',#8390);
#2518=VERTEX_POINT('',#8392);
#2519=VERTEX_POINT('',#8415);
#2520=VERTEX_POINT('',#8417);
#2521=VERTEX_POINT('',#8430);
#2522=VERTEX_POINT('',#8433);
#2523=VERTEX_POINT('',#8446);
#2524=VERTEX_POINT('',#8448);
#2525=VERTEX_POINT('',#8471);
#2526=VERTEX_POINT('',#8473);
#2527=VERTEX_POINT('',#8496);
#2528=VERTEX_POINT('',#8498);
#2529=VERTEX_POINT('',#8521);
#2530=VERTEX_POINT('',#8523);
#2531=VERTEX_POINT('',#8548);
#2532=VERTEX_POINT('',#8552);
#2533=VERTEX_POINT('',#8577);
#2534=VERTEX_POINT('',#8581);
#2535=VERTEX_POINT('',#8606);
#2536=VERTEX_POINT('',#8610);
#2537=VERTEX_POINT('',#8611);
#2538=VERTEX_POINT('',#8638);
#2539=VERTEX_POINT('',#8642);
#2540=VERTEX_POINT('',#8667);
#2541=VERTEX_POINT('',#8671);
#2542=VERTEX_POINT('',#8696);
#2543=VERTEX_POINT('',#8700);
#2544=VERTEX_POINT('',#8725);
#2545=VERTEX_POINT('',#8728);
#2546=VERTEX_POINT('',#8730);
#2547=VERTEX_POINT('',#8762);
#2548=VERTEX_POINT('',#8764);
#2549=VERTEX_POINT('',#8767);
#2550=VERTEX_POINT('',#8771);
#2551=VERTEX_POINT('',#8776);
#2552=VERTEX_POINT('',#8778);
#2553=VERTEX_POINT('',#8781);
#2554=VERTEX_POINT('',#8785);
#2555=VERTEX_POINT('',#8796);
#2556=VERTEX_POINT('',#8797);
#2557=VERTEX_POINT('',#8799);
#2558=VERTEX_POINT('',#8801);
#2559=VERTEX_POINT('',#8805);
#2560=VERTEX_POINT('',#8807);
#2561=VERTEX_POINT('',#8811);
#2562=VERTEX_POINT('',#8813);
#2563=VERTEX_POINT('',#8817);
#2564=VERTEX_POINT('',#8819);
#2565=VERTEX_POINT('',#8823);
#2566=VERTEX_POINT('',#8825);
#2567=VERTEX_POINT('',#8834);
#2568=VERTEX_POINT('',#8837);
#2569=VERTEX_POINT('',#8840);
#2570=VERTEX_POINT('',#8844);
#2571=VERTEX_POINT('',#8848);
#2572=VERTEX_POINT('',#8852);
#2573=VERTEX_POINT('',#8855);
#2574=VERTEX_POINT('',#8862);
#2575=VERTEX_POINT('',#8863);
#2576=VERTEX_POINT('',#8865);
#2577=VERTEX_POINT('',#8867);
#2578=VERTEX_POINT('',#8871);
#2579=VERTEX_POINT('',#8873);
#2580=VERTEX_POINT('',#8877);
#2581=VERTEX_POINT('',#8879);
#2582=VERTEX_POINT('',#8883);
#2583=VERTEX_POINT('',#8885);
#2584=VERTEX_POINT('',#8889);
#2585=VERTEX_POINT('',#8891);
#2586=VERTEX_POINT('',#8900);
#2587=VERTEX_POINT('',#8903);
#2588=VERTEX_POINT('',#8906);
#2589=VERTEX_POINT('',#8910);
#2590=VERTEX_POINT('',#8914);
#2591=VERTEX_POINT('',#8918);
#2592=VERTEX_POINT('',#8921);
#2593=VERTEX_POINT('',#9530);
#2594=VERTEX_POINT('',#9531);
#2595=VERTEX_POINT('',#9599);
#2596=VERTEX_POINT('',#9601);
#2597=VERTEX_POINT('',#9954);
#2598=VERTEX_POINT('',#9956);
#2599=VERTEX_POINT('',#10491);
#2600=VERTEX_POINT('',#10493);
#2601=VERTEX_POINT('',#10496);
#2602=VERTEX_POINT('',#10500);
#2603=VERTEX_POINT('',#10502);
#2604=VERTEX_POINT('',#10507);
#2605=VERTEX_POINT('',#10514);
#2606=VERTEX_POINT('',#10516);
#2607=VERTEX_POINT('',#10520);
#2608=VERTEX_POINT('',#10522);
#2609=VERTEX_POINT('',#10529);
#2610=VERTEX_POINT('',#10530);
#2611=VERTEX_POINT('',#10534);
#2612=VERTEX_POINT('',#10549);
#2613=VERTEX_POINT('',#10551);
#2614=VERTEX_POINT('',#10560);
#2615=VERTEX_POINT('',#10562);
#2616=VERTEX_POINT('',#10610);
#2617=VERTEX_POINT('',#10612);
#2618=VERTEX_POINT('',#10616);
#2619=VERTEX_POINT('',#10618);
#2620=VERTEX_POINT('',#10625);
#2621=VERTEX_POINT('',#10628);
#2622=VERTEX_POINT('',#10629);
#2623=VERTEX_POINT('',#10631);
#2624=VERTEX_POINT('',#10633);
#2625=VERTEX_POINT('',#10637);
#2626=VERTEX_POINT('',#10639);
#2627=VERTEX_POINT('',#10643);
#2628=VERTEX_POINT('',#10645);
#2629=VERTEX_POINT('',#10649);
#2630=VERTEX_POINT('',#10651);
#2631=VERTEX_POINT('',#10655);
#2632=VERTEX_POINT('',#10657);
#2633=VERTEX_POINT('',#10665);
#2634=VERTEX_POINT('',#10668);
#2635=VERTEX_POINT('',#10675);
#2636=VERTEX_POINT('',#10676);
#2637=VERTEX_POINT('',#10680);
#2638=VERTEX_POINT('',#10695);
#2639=VERTEX_POINT('',#10697);
#2640=VERTEX_POINT('',#10699);
#2641=VERTEX_POINT('',#10736);
#2642=VERTEX_POINT('',#10755);
#2643=VERTEX_POINT('',#10757);
#2644=VERTEX_POINT('',#10761);
#2645=VERTEX_POINT('',#10764);
#2646=VERTEX_POINT('',#10768);
#2647=VERTEX_POINT('',#10769);
#2648=VERTEX_POINT('',#10771);
#2649=VERTEX_POINT('',#10773);
#2650=VERTEX_POINT('',#10777);
#2651=VERTEX_POINT('',#10779);
#2652=VERTEX_POINT('',#10783);
#2653=VERTEX_POINT('',#10785);
#2654=VERTEX_POINT('',#10789);
#2655=VERTEX_POINT('',#10791);
#2656=VERTEX_POINT('',#10795);
#2657=VERTEX_POINT('',#10797);
#2658=VERTEX_POINT('',#10801);
#2659=VERTEX_POINT('',#10803);
#2660=VERTEX_POINT('',#10807);
#2661=VERTEX_POINT('',#10809);
#2662=VERTEX_POINT('',#10813);
#2663=VERTEX_POINT('',#10815);
#2664=VERTEX_POINT('',#10819);
#2665=VERTEX_POINT('',#10821);
#2666=VERTEX_POINT('',#10825);
#2667=VERTEX_POINT('',#10827);
#2668=VERTEX_POINT('',#10831);
#2669=VERTEX_POINT('',#10833);
#2670=VERTEX_POINT('',#10837);
#2671=VERTEX_POINT('',#10839);
#2672=VERTEX_POINT('',#10843);
#2673=VERTEX_POINT('',#10845);
#2674=VERTEX_POINT('',#10849);
#2675=VERTEX_POINT('',#10851);
#2676=VERTEX_POINT('',#10855);
#2677=VERTEX_POINT('',#10857);
#2678=VERTEX_POINT('',#10861);
#2679=VERTEX_POINT('',#10863);
#2680=VERTEX_POINT('',#10867);
#2681=VERTEX_POINT('',#10869);
#2682=VERTEX_POINT('',#10873);
#2683=VERTEX_POINT('',#10875);
#2684=VERTEX_POINT('',#10879);
#2685=VERTEX_POINT('',#10881);
#2686=VERTEX_POINT('',#10885);
#2687=VERTEX_POINT('',#10887);
#2688=VERTEX_POINT('',#10891);
#2689=VERTEX_POINT('',#10893);
#2690=VERTEX_POINT('',#10897);
#2691=VERTEX_POINT('',#10899);
#2692=VERTEX_POINT('',#10903);
#2693=VERTEX_POINT('',#10905);
#2694=VERTEX_POINT('',#10909);
#2695=VERTEX_POINT('',#10911);
#2696=VERTEX_POINT('',#10915);
#2697=VERTEX_POINT('',#10917);
#2698=VERTEX_POINT('',#10921);
#2699=VERTEX_POINT('',#10923);
#2700=VERTEX_POINT('',#10927);
#2701=VERTEX_POINT('',#10929);
#2702=VERTEX_POINT('',#10933);
#2703=VERTEX_POINT('',#10935);
#2704=VERTEX_POINT('',#10939);
#2705=VERTEX_POINT('',#10941);
#2706=VERTEX_POINT('',#10945);
#2707=VERTEX_POINT('',#10947);
#2708=VERTEX_POINT('',#10951);
#2709=VERTEX_POINT('',#10953);
#2710=VERTEX_POINT('',#10957);
#2711=VERTEX_POINT('',#10959);
#2712=VERTEX_POINT('',#10963);
#2713=VERTEX_POINT('',#10965);
#2714=VERTEX_POINT('',#10969);
#2715=VERTEX_POINT('',#10971);
#2716=VERTEX_POINT('',#10975);
#2717=VERTEX_POINT('',#10977);
#2718=VERTEX_POINT('',#10981);
#2719=VERTEX_POINT('',#10983);
#2720=VERTEX_POINT('',#10987);
#2721=VERTEX_POINT('',#10989);
#2722=VERTEX_POINT('',#10993);
#2723=VERTEX_POINT('',#10995);
#2724=VERTEX_POINT('',#10999);
#2725=VERTEX_POINT('',#11001);
#2726=VERTEX_POINT('',#11005);
#2727=VERTEX_POINT('',#11007);
#2728=VERTEX_POINT('',#11011);
#2729=VERTEX_POINT('',#11013);
#2730=VERTEX_POINT('',#11017);
#2731=VERTEX_POINT('',#11019);
#2732=VERTEX_POINT('',#11023);
#2733=VERTEX_POINT('',#11025);
#2734=VERTEX_POINT('',#11029);
#2735=VERTEX_POINT('',#11031);
#2736=VERTEX_POINT('',#11035);
#2737=VERTEX_POINT('',#11037);
#2738=VERTEX_POINT('',#11041);
#2739=VERTEX_POINT('',#11043);
#2740=VERTEX_POINT('',#11047);
#2741=VERTEX_POINT('',#11049);
#2742=VERTEX_POINT('',#11059);
#2743=VERTEX_POINT('',#11060);
#2744=VERTEX_POINT('',#11062);
#2745=VERTEX_POINT('',#11064);
#2746=VERTEX_POINT('',#11068);
#2747=VERTEX_POINT('',#11070);
#2748=VERTEX_POINT('',#11074);
#2749=VERTEX_POINT('',#11076);
#2750=VERTEX_POINT('',#11080);
#2751=VERTEX_POINT('',#11082);
#2752=VERTEX_POINT('',#11086);
#2753=VERTEX_POINT('',#11088);
#2754=VERTEX_POINT('',#11096);
#2755=VERTEX_POINT('',#11099);
#2756=VERTEX_POINT('',#11103);
#2757=VERTEX_POINT('',#11107);
#2758=VERTEX_POINT('',#11120);
#2759=VERTEX_POINT('',#11121);
#2760=VERTEX_POINT('',#11123);
#2761=VERTEX_POINT('',#11125);
#2762=VERTEX_POINT('',#11129);
#2763=VERTEX_POINT('',#11131);
#2764=VERTEX_POINT('',#11133);
#2765=VERTEX_POINT('',#11135);
#2766=VERTEX_POINT('',#11137);
#2767=VERTEX_POINT('',#11140);
#2768=VERTEX_POINT('',#11143);
#2769=VERTEX_POINT('',#11145);
#2770=VERTEX_POINT('',#11147);
#2771=VERTEX_POINT('',#11154);
#2772=VERTEX_POINT('',#11157);
#2773=VERTEX_POINT('',#11159);
#2774=VERTEX_POINT('',#11163);
#2775=VERTEX_POINT('',#11166);
#2776=VERTEX_POINT('',#11175);
#2777=VERTEX_POINT('',#11179);
#2778=VERTEX_POINT('',#11181);
#2779=VERTEX_POINT('',#11185);
#2780=VERTEX_POINT('',#11189);
#2781=EDGE_CURVE('',#2335,#2335,#2091,.T.);
#2782=EDGE_CURVE('',#2335,#2336,#1325,.T.);
#2783=EDGE_CURVE('',#2336,#2336,#2092,.T.);
#2784=EDGE_CURVE('',#2337,#2337,#2093,.T.);
#2785=EDGE_CURVE('',#2337,#2338,#1326,.T.);
#2786=EDGE_CURVE('',#2338,#2338,#2094,.T.);
#2787=EDGE_CURVE('',#2339,#2339,#2095,.T.);
#2788=EDGE_CURVE('',#2339,#2340,#1327,.T.);
#2789=EDGE_CURVE('',#2340,#2340,#2096,.T.);
#2790=EDGE_CURVE('',#2341,#2341,#2097,.T.);
#2791=EDGE_CURVE('',#2341,#2342,#1328,.T.);
#2792=EDGE_CURVE('',#2342,#2342,#2098,.T.);
#2793=EDGE_CURVE('',#2343,#2343,#2099,.T.);
#2794=EDGE_CURVE('',#2343,#2344,#1329,.T.);
#2795=EDGE_CURVE('',#2344,#2344,#2100,.T.);
#2796=EDGE_CURVE('',#2345,#2345,#2101,.T.);
#2797=EDGE_CURVE('',#2345,#2346,#1330,.T.);
#2798=EDGE_CURVE('',#2346,#2346,#2102,.T.);
#2799=EDGE_CURVE('',#2347,#2347,#2103,.T.);
#2800=EDGE_CURVE('',#2347,#2348,#1331,.T.);
#2801=EDGE_CURVE('',#2348,#2348,#2104,.T.);
#2802=EDGE_CURVE('',#2349,#2350,#1332,.T.);
#2803=EDGE_CURVE('',#2350,#2351,#1333,.T.);
#2804=EDGE_CURVE('',#2352,#2351,#1334,.T.);
#2805=EDGE_CURVE('',#2349,#2352,#1335,.T.);
#2806=EDGE_CURVE('',#2353,#2349,#1336,.T.);
#2807=EDGE_CURVE('',#2354,#2352,#1337,.T.);
#2808=EDGE_CURVE('',#2353,#2354,#1338,.T.);
#2809=EDGE_CURVE('',#2355,#2353,#1339,.T.);
#2810=EDGE_CURVE('',#2356,#2354,#1340,.T.);
#2811=EDGE_CURVE('',#2355,#2356,#1341,.T.);
#2812=EDGE_CURVE('',#2350,#2355,#1342,.T.);
#2813=EDGE_CURVE('',#2351,#2356,#1343,.T.);
#2814=EDGE_CURVE('',#2357,#2357,#2105,.T.);
#2815=EDGE_CURVE('',#2357,#2358,#1344,.T.);
#2816=EDGE_CURVE('',#2358,#2358,#2106,.T.);
#2817=EDGE_CURVE('',#2359,#2359,#2107,.T.);
#2818=EDGE_CURVE('',#2359,#2360,#1345,.T.);
#2819=EDGE_CURVE('',#2360,#2360,#2108,.T.);
#2820=EDGE_CURVE('',#2361,#2361,#2109,.T.);
#2821=EDGE_CURVE('',#2361,#2362,#1346,.T.);
#2822=EDGE_CURVE('',#2362,#2362,#2110,.T.);
#2823=EDGE_CURVE('',#2363,#2363,#2111,.T.);
#2824=EDGE_CURVE('',#2363,#2364,#1347,.T.);
#2825=EDGE_CURVE('',#2364,#2364,#2112,.T.);
#2826=EDGE_CURVE('',#2365,#2365,#2113,.T.);
#2827=EDGE_CURVE('',#2365,#2366,#1348,.T.);
#2828=EDGE_CURVE('',#2366,#2366,#2114,.T.);
#2829=EDGE_CURVE('',#2367,#2368,#1349,.T.);
#2830=EDGE_CURVE('',#2368,#2369,#1350,.T.);
#2831=EDGE_CURVE('',#2370,#2369,#1351,.T.);
#2832=EDGE_CURVE('',#2367,#2370,#1352,.T.);
#2833=EDGE_CURVE('',#2371,#2367,#1353,.T.);
#2834=EDGE_CURVE('',#2372,#2370,#1354,.T.);
#2835=EDGE_CURVE('',#2371,#2372,#1355,.T.);
#2836=EDGE_CURVE('',#2373,#2371,#1356,.T.);
#2837=EDGE_CURVE('',#2374,#2372,#1357,.T.);
#2838=EDGE_CURVE('',#2373,#2374,#1358,.T.);
#2839=EDGE_CURVE('',#2368,#2373,#1359,.T.);
#2840=EDGE_CURVE('',#2369,#2374,#1360,.T.);
#2841=EDGE_CURVE('',#2375,#2375,#2115,.T.);
#2842=EDGE_CURVE('',#2375,#2376,#1361,.T.);
#2843=EDGE_CURVE('',#2376,#2376,#2116,.T.);
#2844=EDGE_CURVE('',#2377,#2377,#2117,.T.);
#2845=EDGE_CURVE('',#2378,#2378,#2118,.T.);
#2846=EDGE_CURVE('',#2377,#2379,#1362,.T.);
#2847=EDGE_CURVE('',#2379,#2379,#2119,.T.);
#2848=EDGE_CURVE('',#2380,#2380,#2120,.T.);
#2849=EDGE_CURVE('',#2380,#2378,#1363,.T.);
#2850=EDGE_CURVE('',#2381,#2381,#2121,.T.);
#2851=EDGE_CURVE('',#2381,#2382,#1364,.T.);
#2852=EDGE_CURVE('',#2382,#2382,#2122,.T.);
#2853=EDGE_CURVE('',#2383,#2383,#2123,.T.);
#2854=EDGE_CURVE('',#2383,#2384,#1365,.T.);
#2855=EDGE_CURVE('',#2384,#2384,#2124,.T.);
#2856=EDGE_CURVE('',#2385,#2385,#2125,.T.);
#2857=EDGE_CURVE('',#2385,#2386,#1366,.T.);
#2858=EDGE_CURVE('',#2386,#2386,#2126,.T.);
#2859=EDGE_CURVE('',#2387,#2387,#2127,.T.);
#2860=EDGE_CURVE('',#2387,#2388,#1367,.T.);
#2861=EDGE_CURVE('',#2388,#2388,#2128,.T.);
#2862=EDGE_CURVE('',#2389,#2389,#2129,.T.);
#2863=EDGE_CURVE('',#2389,#2390,#1368,.T.);
#2864=EDGE_CURVE('',#2390,#2390,#2130,.T.);
#2865=EDGE_CURVE('',#2391,#2391,#2131,.T.);
#2866=EDGE_CURVE('',#2391,#2392,#1369,.T.);
#2867=EDGE_CURVE('',#2392,#2392,#2132,.T.);
#2868=EDGE_CURVE('',#2393,#2393,#2133,.T.);
#2869=EDGE_CURVE('',#2393,#2394,#1370,.T.);
#2870=EDGE_CURVE('',#2394,#2394,#2134,.T.);
#2871=EDGE_CURVE('',#2395,#2395,#2135,.T.);
#2872=EDGE_CURVE('',#2395,#2396,#1371,.T.);
#2873=EDGE_CURVE('',#2397,#2396,#2136,.T.);
#2874=EDGE_CURVE('',#2396,#2397,#2137,.T.);
#2875=EDGE_CURVE('',#2398,#2399,#1372,.T.);
#2876=EDGE_CURVE('',#2399,#2397,#1373,.T.);
#2877=EDGE_CURVE('',#2397,#2400,#1374,.T.);
#2878=EDGE_CURVE('',#2400,#2401,#1375,.T.);
#2879=EDGE_CURVE('',#2401,#2398,#1376,.T.);
#2880=EDGE_CURVE('',#2402,#2403,#1377,.T.);
#2881=EDGE_CURVE('',#2404,#2402,#1378,.T.);
#2882=EDGE_CURVE('',#2405,#2404,#1379,.T.);
#2883=EDGE_CURVE('',#2405,#2406,#2138,.T.);
#2884=EDGE_CURVE('',#2406,#2405,#2139,.T.);
#2885=EDGE_CURVE('',#2407,#2405,#1380,.T.);
#2886=EDGE_CURVE('',#2403,#2407,#1381,.T.);
#2887=EDGE_CURVE('',#2402,#2398,#1382,.T.);
#2888=EDGE_CURVE('',#2404,#2401,#1383,.T.);
#2889=EDGE_CURVE('',#2407,#2400,#1384,.T.);
#2890=EDGE_CURVE('',#2403,#2399,#1385,.T.);
#2891=EDGE_CURVE('',#2406,#2408,#1386,.T.);
#2892=EDGE_CURVE('',#2408,#2408,#2140,.T.);
#2893=EDGE_CURVE('',#2409,#2410,#201,.T.);
#2894=EDGE_CURVE('',#2410,#2409,#202,.T.);
#2895=EDGE_CURVE('',#2410,#2411,#1387,.T.);
#2896=EDGE_CURVE('',#2412,#2411,#203,.T.);
#2897=EDGE_CURVE('',#2411,#2412,#204,.T.);
#2898=EDGE_CURVE('',#2413,#2413,#2141,.T.);
#2899=EDGE_CURVE('',#2413,#2414,#1388,.T.);
#2900=EDGE_CURVE('',#2414,#2414,#2142,.T.);
#2901=EDGE_CURVE('',#2415,#2415,#2143,.T.);
#2902=EDGE_CURVE('',#2415,#2416,#1389,.T.);
#2903=EDGE_CURVE('',#2416,#2416,#2144,.T.);
#2904=EDGE_CURVE('',#2417,#2417,#2145,.T.);
#2905=EDGE_CURVE('',#2417,#2418,#1390,.T.);
#2906=EDGE_CURVE('',#2418,#2418,#2146,.T.);
#2907=EDGE_CURVE('',#2419,#2419,#2147,.T.);
#2908=EDGE_CURVE('',#2419,#2420,#1391,.T.);
#2909=EDGE_CURVE('',#2420,#2420,#2148,.T.);
#2910=EDGE_CURVE('',#2421,#2422,#2149,.T.);
#2911=EDGE_CURVE('',#2422,#2421,#2150,.T.);
#2912=EDGE_CURVE('',#2423,#2421,#1392,.T.);
#2913=EDGE_CURVE('',#2424,#2423,#2151,.T.);
#2914=EDGE_CURVE('',#2422,#2424,#1393,.T.);
#2915=EDGE_CURVE('',#2425,#2426,#1394,.T.);
#2916=EDGE_CURVE('',#2425,#2427,#2152,.T.);
#2917=EDGE_CURVE('',#2428,#2427,#1395,.T.);
#2918=EDGE_CURVE('',#2426,#2428,#2153,.T.);
#2919=EDGE_CURVE('',#2427,#2425,#2154,.T.);
#2920=EDGE_CURVE('',#2429,#2430,#1396,.T.);
#2921=EDGE_CURVE('',#2429,#2431,#2155,.T.);
#2922=EDGE_CURVE('',#2432,#2431,#1397,.T.);
#2923=EDGE_CURVE('',#2430,#2432,#2156,.T.);
#2924=EDGE_CURVE('',#2431,#2429,#2157,.T.);
#2925=EDGE_CURVE('',#2433,#2434,#1398,.T.);
#2926=EDGE_CURVE('',#2433,#2435,#2158,.T.);
#2927=EDGE_CURVE('',#2436,#2435,#1399,.T.);
#2928=EDGE_CURVE('',#2434,#2436,#2159,.T.);
#2929=EDGE_CURVE('',#2435,#2433,#2160,.T.);
#2930=EDGE_CURVE('',#2437,#2437,#2161,.T.);
#2931=EDGE_CURVE('',#2437,#2438,#1400,.T.);
#2932=EDGE_CURVE('',#2438,#2423,#2162,.T.);
#2933=EDGE_CURVE('',#2424,#2436,#2163,.T.);
#2934=EDGE_CURVE('',#2434,#2432,#2164,.T.);
#2935=EDGE_CURVE('',#2430,#2428,#2165,.T.);
#2936=EDGE_CURVE('',#2426,#2438,#2166,.T.);
#2937=EDGE_CURVE('',#2439,#2439,#2167,.T.);
#2938=EDGE_CURVE('',#2440,#2440,#2168,.T.);
#2939=EDGE_CURVE('',#2441,#2441,#2169,.T.);
#2940=EDGE_CURVE('',#2442,#2442,#2170,.T.);
#2941=EDGE_CURVE('',#2443,#2443,#2171,.T.);
#2942=EDGE_CURVE('',#2444,#2444,#2172,.T.);
#2943=EDGE_CURVE('',#2444,#2440,#1401,.T.);
#2944=EDGE_CURVE('',#2445,#2445,#2173,.T.);
#2945=EDGE_CURVE('',#2445,#2443,#1402,.T.);
#2946=EDGE_CURVE('',#2446,#2446,#2174,.T.);
#2947=EDGE_CURVE('',#2446,#2441,#1403,.T.);
#2948=EDGE_CURVE('',#2447,#2447,#2175,.T.);
#2949=EDGE_CURVE('',#2447,#2442,#1404,.T.);
#2950=EDGE_CURVE('',#2448,#2448,#2176,.T.);
#2951=EDGE_CURVE('',#2448,#2449,#1405,.T.);
#2952=EDGE_CURVE('',#2449,#2449,#2177,.T.);
#2953=EDGE_CURVE('',#2450,#2450,#2178,.T.);
#2954=EDGE_CURVE('',#2439,#2451,#1406,.T.);
#2955=EDGE_CURVE('',#2451,#2451,#2179,.T.);
#2956=EDGE_CURVE('',#2450,#2452,#1407,.T.);
#2957=EDGE_CURVE('',#2452,#2452,#2180,.T.);
#2958=EDGE_CURVE('',#2453,#2453,#2181,.T.);
#2959=EDGE_CURVE('',#2453,#2454,#1408,.T.);
#2960=EDGE_CURVE('',#2454,#2454,#2182,.T.);
#2961=EDGE_CURVE('',#2455,#2455,#2183,.T.);
#2962=EDGE_CURVE('',#2456,#2456,#2184,.T.);
#2963=EDGE_CURVE('',#2456,#2457,#1409,.T.);
#2964=EDGE_CURVE('',#2457,#2457,#2185,.T.);
#2965=EDGE_CURVE('',#2458,#2458,#2186,.T.);
#2966=EDGE_CURVE('',#2459,#2459,#2187,.T.);
#2967=EDGE_CURVE('',#2459,#2460,#1410,.T.);
#2968=EDGE_CURVE('',#2460,#2460,#2188,.T.);
#2969=EDGE_CURVE('',#2461,#2461,#2189,.T.);
#2970=EDGE_CURVE('',#2462,#2462,#2190,.T.);
#2971=EDGE_CURVE('',#2462,#2463,#1411,.T.);
#2972=EDGE_CURVE('',#2463,#2463,#2191,.T.);
#2973=EDGE_CURVE('',#2464,#2464,#2192,.T.);
#2974=EDGE_CURVE('',#2465,#2465,#2193,.T.);
#2975=EDGE_CURVE('',#2465,#2455,#1412,.T.);
#2976=EDGE_CURVE('',#2466,#2466,#2194,.T.);
#2977=EDGE_CURVE('',#2466,#2458,#1413,.T.);
#2978=EDGE_CURVE('',#2467,#2467,#2195,.T.);
#2979=EDGE_CURVE('',#2467,#2461,#1414,.T.);
#2980=EDGE_CURVE('',#2468,#2468,#2196,.T.);
#2981=EDGE_CURVE('',#2468,#2464,#1415,.T.);
#2982=EDGE_CURVE('',#2469,#2469,#2197,.T.);
#2983=EDGE_CURVE('',#2469,#2470,#1416,.T.);
#2984=EDGE_CURVE('',#2470,#2470,#2198,.T.);
#2985=EDGE_CURVE('',#2471,#2471,#2199,.T.);
#2986=EDGE_CURVE('',#2472,#2472,#2200,.T.);
#2987=EDGE_CURVE('',#2472,#2471,#1417,.T.);
#2988=EDGE_CURVE('',#2473,#2473,#2201,.T.);
#2989=EDGE_CURVE('',#2473,#2474,#1418,.T.);
#2990=EDGE_CURVE('',#2474,#2474,#2202,.T.);
#2991=EDGE_CURVE('',#2475,#2476,#2203,.T.);
#2992=EDGE_CURVE('',#2476,#2475,#2204,.T.);
#2993=EDGE_CURVE('',#2476,#2477,#2205,.T.);
#2994=EDGE_CURVE('',#2478,#2477,#2206,.T.);
#2995=EDGE_CURVE('',#2477,#2478,#2207,.T.);
#2996=EDGE_CURVE('',#2478,#2479,#1419,.T.);
#2997=EDGE_CURVE('',#2479,#2479,#2208,.T.);
#2998=EDGE_CURVE('',#2480,#2480,#2209,.T.);
#2999=EDGE_CURVE('',#2480,#2481,#1420,.T.);
#3000=EDGE_CURVE('',#2481,#2481,#2210,.T.);
#3001=EDGE_CURVE('',#2481,#2482,#1421,.T.);
#3002=EDGE_CURVE('',#2482,#2482,#2211,.T.);
#3003=EDGE_CURVE('',#2483,#2483,#2212,.T.);
#3004=EDGE_CURVE('',#2483,#2475,#1422,.T.);
#3005=EDGE_CURVE('',#2484,#2484,#2213,.T.);
#3006=EDGE_CURVE('',#2484,#2480,#1423,.T.);
#3007=EDGE_CURVE('',#2485,#2486,#2214,.T.);
#3008=EDGE_CURVE('',#2486,#2485,#2215,.T.);
#3009=EDGE_CURVE('',#2486,#2487,#2216,.T.);
#3010=EDGE_CURVE('',#2488,#2487,#2217,.T.);
#3011=EDGE_CURVE('',#2487,#2488,#2218,.T.);
#3012=EDGE_CURVE('',#2489,#2489,#2219,.T.);
#3013=EDGE_CURVE('',#2489,#2488,#1424,.T.);
#3014=EDGE_CURVE('',#2490,#2490,#2220,.T.);
#3015=EDGE_CURVE('',#2491,#2491,#2221,.T.);
#3016=EDGE_CURVE('',#2492,#2492,#2222,.T.);
#3017=EDGE_CURVE('',#2492,#2490,#1425,.T.);
#3018=EDGE_CURVE('',#2493,#2493,#2223,.T.);
#3019=EDGE_CURVE('',#2493,#2492,#1426,.T.);
#3020=EDGE_CURVE('',#2494,#2494,#2224,.T.);
#3021=EDGE_CURVE('',#2494,#2493,#1427,.T.);
#3022=EDGE_CURVE('',#2485,#2491,#1428,.T.);
#3023=EDGE_CURVE('',#2495,#2496,#2225,.T.);
#3024=EDGE_CURVE('',#2497,#2498,#2226,.T.);
#3025=EDGE_CURVE('',#2499,#2500,#2227,.T.);
#3026=EDGE_CURVE('',#2501,#2502,#2228,.T.);
#3027=EDGE_CURVE('',#2503,#2504,#2229,.T.);
#3028=EDGE_CURVE('',#2505,#2506,#2230,.T.);
#3029=EDGE_CURVE('',#2507,#2508,#2231,.T.);
#3030=EDGE_CURVE('',#2509,#2510,#2232,.T.);
#3031=EDGE_CURVE('',#2511,#2512,#205,.T.);
#3032=EDGE_CURVE('',#2513,#2511,#2233,.T.);
#3033=EDGE_CURVE('',#2514,#2513,#206,.T.);
#3034=EDGE_CURVE('',#2512,#2514,#2234,.T.);
#3035=EDGE_CURVE('',#2515,#2513,#2235,.T.);
#3036=EDGE_CURVE('',#2515,#2516,#207,.T.);
#3037=EDGE_CURVE('',#2517,#2516,#2236,.T.);
#3038=EDGE_CURVE('',#2517,#2518,#208,.T.);
#3039=EDGE_CURVE('',#2519,#2518,#2237,.T.);
#3040=EDGE_CURVE('',#2519,#2520,#209,.T.);
#3041=EDGE_CURVE('',#2520,#2521,#1429,.T.);
#3042=EDGE_CURVE('',#2521,#2521,#2238,.T.);
#3043=EDGE_CURVE('',#2520,#2522,#210,.T.);
#3044=EDGE_CURVE('',#2523,#2522,#2239,.T.);
#3045=EDGE_CURVE('',#2523,#2524,#211,.T.);
#3046=EDGE_CURVE('',#2525,#2524,#2240,.T.);
#3047=EDGE_CURVE('',#2525,#2526,#212,.T.);
#3048=EDGE_CURVE('',#2527,#2526,#2241,.T.);
#3049=EDGE_CURVE('',#2527,#2528,#213,.T.);
#3050=EDGE_CURVE('',#2529,#2528,#2242,.T.);
#3051=EDGE_CURVE('',#2529,#2530,#214,.T.);
#3052=EDGE_CURVE('',#2514,#2530,#2243,.T.);
#3053=EDGE_CURVE('',#2511,#2531,#2244,.T.);
#3054=EDGE_CURVE('',#2531,#2515,#2245,.T.);
#3055=EDGE_CURVE('',#2532,#2531,#215,.T.);
#3056=EDGE_CURVE('',#2516,#2532,#2246,.T.);
#3057=EDGE_CURVE('',#2532,#2533,#2247,.T.);
#3058=EDGE_CURVE('',#2533,#2517,#2248,.T.);
#3059=EDGE_CURVE('',#2534,#2533,#216,.T.);
#3060=EDGE_CURVE('',#2518,#2534,#2249,.T.);
#3061=EDGE_CURVE('',#2534,#2535,#2250,.T.);
#3062=EDGE_CURVE('',#2535,#2519,#2251,.T.);
#3063=EDGE_CURVE('',#2536,#2537,#217,.T.);
#3064=EDGE_CURVE('',#2522,#2536,#2252,.T.);
#3065=EDGE_CURVE('',#2537,#2535,#218,.T.);
#3066=EDGE_CURVE('',#2536,#2538,#2253,.T.);
#3067=EDGE_CURVE('',#2538,#2523,#2254,.T.);
#3068=EDGE_CURVE('',#2539,#2538,#219,.T.);
#3069=EDGE_CURVE('',#2524,#2539,#2255,.T.);
#3070=EDGE_CURVE('',#2539,#2540,#2256,.T.);
#3071=EDGE_CURVE('',#2540,#2525,#2257,.T.);
#3072=EDGE_CURVE('',#2541,#2540,#220,.T.);
#3073=EDGE_CURVE('',#2526,#2541,#2258,.T.);
#3074=EDGE_CURVE('',#2541,#2542,#2259,.T.);
#3075=EDGE_CURVE('',#2542,#2527,#2260,.T.);
#3076=EDGE_CURVE('',#2543,#2542,#221,.T.);
#3077=EDGE_CURVE('',#2528,#2543,#2261,.T.);
#3078=EDGE_CURVE('',#2544,#2544,#2262,.T.);
#3079=EDGE_CURVE('',#2544,#2537,#1430,.T.);
#3080=EDGE_CURVE('',#2545,#2512,#2263,.T.);
#3081=EDGE_CURVE('',#2545,#2546,#222,.T.);
#3082=EDGE_CURVE('',#2543,#2546,#2264,.T.);
#3083=EDGE_CURVE('',#2530,#2545,#2265,.T.);
#3084=EDGE_CURVE('',#2546,#2529,#2266,.T.);
#3085=EDGE_CURVE('',#2547,#2547,#2267,.T.);
#3086=EDGE_CURVE('',#2548,#2548,#2268,.T.);
#3087=EDGE_CURVE('',#2549,#2549,#2269,.T.);
#3088=EDGE_CURVE('',#2549,#2547,#1431,.T.);
#3089=EDGE_CURVE('',#2550,#2550,#2270,.T.);
#3090=EDGE_CURVE('',#2550,#2548,#1432,.T.);
#3091=EDGE_CURVE('',#2551,#2551,#2271,.T.);
#3092=EDGE_CURVE('',#2552,#2552,#2272,.T.);
#3093=EDGE_CURVE('',#2553,#2553,#2273,.T.);
#3094=EDGE_CURVE('',#2553,#2551,#1433,.T.);
#3095=EDGE_CURVE('',#2554,#2554,#2274,.T.);
#3096=EDGE_CURVE('',#2554,#2552,#1434,.T.);
#3097=EDGE_CURVE('',#2555,#2556,#1435,.T.);
#3098=EDGE_CURVE('',#2556,#2557,#1436,.T.);
#3099=EDGE_CURVE('',#2557,#2558,#1437,.T.);
#3100=EDGE_CURVE('',#2555,#2558,#1438,.T.);
#3101=EDGE_CURVE('',#2556,#2559,#1439,.T.);
#3102=EDGE_CURVE('',#2559,#2560,#1440,.T.);
#3103=EDGE_CURVE('',#2560,#2557,#1441,.T.);
#3104=EDGE_CURVE('',#2559,#2561,#1442,.T.);
#3105=EDGE_CURVE('',#2561,#2562,#1443,.T.);
#3106=EDGE_CURVE('',#2562,#2560,#1444,.T.);
#3107=EDGE_CURVE('',#2561,#2563,#1445,.T.);
#3108=EDGE_CURVE('',#2563,#2564,#1446,.T.);
#3109=EDGE_CURVE('',#2564,#2562,#1447,.T.);
#3110=EDGE_CURVE('',#2563,#2565,#1448,.T.);
#3111=EDGE_CURVE('',#2565,#2566,#1449,.T.);
#3112=EDGE_CURVE('',#2566,#2564,#1450,.T.);
#3113=EDGE_CURVE('',#2565,#2555,#1451,.T.);
#3114=EDGE_CURVE('',#2558,#2566,#1452,.T.);
#3115=EDGE_CURVE('',#2567,#2567,#2275,.T.);
#3116=EDGE_CURVE('',#2568,#2568,#2276,.T.);
#3117=EDGE_CURVE('',#2569,#2569,#2277,.T.);
#3118=EDGE_CURVE('',#2569,#2568,#1453,.T.);
#3119=EDGE_CURVE('',#2570,#2570,#2278,.T.);
#3120=EDGE_CURVE('',#2570,#2569,#1454,.T.);
#3121=EDGE_CURVE('',#2571,#2571,#2279,.T.);
#3122=EDGE_CURVE('',#2571,#2570,#1455,.T.);
#3123=EDGE_CURVE('',#2572,#2572,#2280,.T.);
#3124=EDGE_CURVE('',#2573,#2573,#2281,.F.);
#3125=EDGE_CURVE('',#2573,#2572,#1456,.T.);
#3126=EDGE_CURVE('',#2567,#2573,#1457,.T.);
#3127=EDGE_CURVE('',#2574,#2575,#1458,.T.);
#3128=EDGE_CURVE('',#2575,#2576,#1459,.T.);
#3129=EDGE_CURVE('',#2576,#2577,#1460,.T.);
#3130=EDGE_CURVE('',#2574,#2577,#1461,.T.);
#3131=EDGE_CURVE('',#2575,#2578,#1462,.T.);
#3132=EDGE_CURVE('',#2578,#2579,#1463,.T.);
#3133=EDGE_CURVE('',#2579,#2576,#1464,.T.);
#3134=EDGE_CURVE('',#2578,#2580,#1465,.T.);
#3135=EDGE_CURVE('',#2580,#2581,#1466,.T.);
#3136=EDGE_CURVE('',#2581,#2579,#1467,.T.);
#3137=EDGE_CURVE('',#2580,#2582,#1468,.T.);
#3138=EDGE_CURVE('',#2582,#2583,#1469,.T.);
#3139=EDGE_CURVE('',#2583,#2581,#1470,.T.);
#3140=EDGE_CURVE('',#2582,#2584,#1471,.T.);
#3141=EDGE_CURVE('',#2584,#2585,#1472,.T.);
#3142=EDGE_CURVE('',#2585,#2583,#1473,.T.);
#3143=EDGE_CURVE('',#2584,#2574,#1474,.T.);
#3144=EDGE_CURVE('',#2577,#2585,#1475,.T.);
#3145=EDGE_CURVE('',#2586,#2586,#2282,.T.);
#3146=EDGE_CURVE('',#2587,#2587,#2283,.T.);
#3147=EDGE_CURVE('',#2588,#2588,#2284,.T.);
#3148=EDGE_CURVE('',#2588,#2587,#1476,.T.);
#3149=EDGE_CURVE('',#2589,#2589,#2285,.T.);
#3150=EDGE_CURVE('',#2589,#2588,#1477,.T.);
#3151=EDGE_CURVE('',#2590,#2590,#2286,.T.);
#3152=EDGE_CURVE('',#2590,#2589,#1478,.T.);
#3153=EDGE_CURVE('',#2591,#2591,#2287,.T.);
#3154=EDGE_CURVE('',#2592,#2592,#2288,.F.);
#3155=EDGE_CURVE('',#2592,#2591,#1479,.T.);
#3156=EDGE_CURVE('',#2586,#2592,#1480,.T.);
#3157=EDGE_CURVE('',#2593,#2594,#223,.T.);
#3158=EDGE_CURVE('',#2595,#2593,#2289,.T.);
#3159=EDGE_CURVE('',#2595,#2596,#224,.T.);
#3160=EDGE_CURVE('',#2596,#2594,#2290,.T.);
#3161=EDGE_CURVE('',#2597,#2595,#2291,.T.);
#3162=EDGE_CURVE('',#2598,#2597,#225,.T.);
#3163=EDGE_CURVE('',#2598,#2596,#2292,.T.);
#3164=EDGE_CURVE('',#2594,#2598,#2293,.T.);
#3165=EDGE_CURVE('',#2593,#2597,#2294,.T.);
#3166=EDGE_CURVE('',#2599,#2599,#2295,.T.);
#3167=EDGE_CURVE('',#2600,#2600,#2296,.T.);
#3168=EDGE_CURVE('',#2601,#2601,#2297,.T.);
#3169=EDGE_CURVE('',#2601,#2599,#1481,.T.);
#3170=EDGE_CURVE('',#2602,#2602,#2298,.T.);
#3171=EDGE_CURVE('',#2603,#2603,#2299,.T.);
#3172=EDGE_CURVE('',#2600,#2602,#1482,.T.);
#3173=EDGE_CURVE('',#2603,#2604,#1483,.T.);
#3174=EDGE_CURVE('',#2604,#2604,#2300,.T.);
#3175=EDGE_CURVE('',#2605,#2605,#2301,.T.);
#3176=EDGE_CURVE('',#2605,#2606,#1484,.T.);
#3177=EDGE_CURVE('',#2606,#2606,#2302,.T.);
#3178=EDGE_CURVE('',#2607,#2607,#2303,.T.);
#3179=EDGE_CURVE('',#2607,#2608,#1485,.T.);
#3180=EDGE_CURVE('',#2608,#2608,#2304,.T.);
#3181=EDGE_CURVE('',#2609,#2610,#1486,.T.);
#3182=EDGE_CURVE('',#2609,#2610,#2305,.T.);
#3183=EDGE_CURVE('',#2611,#2609,#226,.T.);
#3184=EDGE_CURVE('',#2612,#2611,#2306,.T.);
#3185=EDGE_CURVE('',#2613,#2612,#227,.T.);
#3186=EDGE_CURVE('',#2613,#2614,#1487,.T.);
#3187=EDGE_CURVE('',#2615,#2614,#228,.T.);
#3188=EDGE_CURVE('',#2614,#2615,#229,.T.);
#3189=EDGE_CURVE('',#2610,#2613,#230,.T.);
#3190=EDGE_CURVE('',#2612,#2611,#1488,.T.);
#3191=EDGE_CURVE('',#2616,#2616,#2307,.T.);
#3192=EDGE_CURVE('',#2616,#2617,#1489,.T.);
#3193=EDGE_CURVE('',#2617,#2617,#2308,.T.);
#3194=EDGE_CURVE('',#2618,#2618,#2309,.T.);
#3195=EDGE_CURVE('',#2618,#2619,#1490,.T.);
#3196=EDGE_CURVE('',#2619,#2619,#2310,.T.);
#3197=EDGE_CURVE('',#2620,#2620,#2311,.T.);
#3198=EDGE_CURVE('',#2621,#2622,#1491,.T.);
#3199=EDGE_CURVE('',#2621,#2623,#1492,.T.);
#3200=EDGE_CURVE('',#2623,#2624,#1493,.T.);
#3201=EDGE_CURVE('',#2622,#2624,#1494,.T.);
#3202=EDGE_CURVE('',#2625,#2621,#1495,.T.);
#3203=EDGE_CURVE('',#2625,#2626,#1496,.T.);
#3204=EDGE_CURVE('',#2626,#2623,#1497,.T.);
#3205=EDGE_CURVE('',#2627,#2625,#1498,.T.);
#3206=EDGE_CURVE('',#2627,#2628,#1499,.T.);
#3207=EDGE_CURVE('',#2628,#2626,#1500,.T.);
#3208=EDGE_CURVE('',#2629,#2627,#1501,.T.);
#3209=EDGE_CURVE('',#2629,#2630,#1502,.T.);
#3210=EDGE_CURVE('',#2630,#2628,#1503,.T.);
#3211=EDGE_CURVE('',#2631,#2629,#1504,.T.);
#3212=EDGE_CURVE('',#2631,#2632,#1505,.T.);
#3213=EDGE_CURVE('',#2632,#2630,#1506,.T.);
#3214=EDGE_CURVE('',#2622,#2631,#1507,.T.);
#3215=EDGE_CURVE('',#2624,#2632,#1508,.T.);
#3216=EDGE_CURVE('',#2633,#2633,#2312,.T.);
#3217=EDGE_CURVE('',#2634,#2634,#2313,.T.);
#3218=EDGE_CURVE('',#2634,#2633,#1509,.T.);
#3219=EDGE_CURVE('',#2620,#2634,#1510,.T.);
#3220=EDGE_CURVE('',#2635,#2636,#1511,.T.);
#3221=EDGE_CURVE('',#2635,#2636,#2314,.T.);
#3222=EDGE_CURVE('',#2637,#2635,#231,.T.);
#3223=EDGE_CURVE('',#2638,#2637,#2315,.T.);
#3224=EDGE_CURVE('',#2638,#2639,#1512,.T.);
#3225=EDGE_CURVE('',#2640,#2639,#232,.T.);
#3226=EDGE_CURVE('',#2639,#2640,#233,.T.);
#3227=EDGE_CURVE('',#2641,#2638,#2316,.T.);
#3228=EDGE_CURVE('',#2636,#2641,#234,.T.);
#3229=EDGE_CURVE('',#2641,#2637,#1513,.T.);
#3230=EDGE_CURVE('',#2642,#2642,#2317,.T.);
#3231=EDGE_CURVE('',#2642,#2643,#1514,.T.);
#3232=EDGE_CURVE('',#2643,#2643,#2318,.T.);
#3233=EDGE_CURVE('',#2644,#2644,#2319,.T.);
#3234=EDGE_CURVE('',#2645,#2645,#2320,.T.);
#3235=EDGE_CURVE('',#2645,#2644,#1515,.T.);
#3236=EDGE_CURVE('',#2646,#2647,#1516,.T.);
#3237=EDGE_CURVE('',#2646,#2648,#1517,.T.);
#3238=EDGE_CURVE('',#2649,#2648,#1518,.T.);
#3239=EDGE_CURVE('',#2647,#2649,#1519,.T.);
#3240=EDGE_CURVE('',#2647,#2650,#1520,.T.);
#3241=EDGE_CURVE('',#2651,#2649,#1521,.T.);
#3242=EDGE_CURVE('',#2650,#2651,#1522,.T.);
#3243=EDGE_CURVE('',#2650,#2652,#1523,.T.);
#3244=EDGE_CURVE('',#2653,#2651,#1524,.T.);
#3245=EDGE_CURVE('',#2652,#2653,#1525,.T.);
#3246=EDGE_CURVE('',#2652,#2654,#1526,.T.);
#3247=EDGE_CURVE('',#2655,#2653,#1527,.T.);
#3248=EDGE_CURVE('',#2654,#2655,#1528,.T.);
#3249=EDGE_CURVE('',#2654,#2656,#1529,.T.);
#3250=EDGE_CURVE('',#2657,#2655,#1530,.T.);
#3251=EDGE_CURVE('',#2656,#2657,#1531,.T.);
#3252=EDGE_CURVE('',#2656,#2658,#1532,.T.);
#3253=EDGE_CURVE('',#2659,#2657,#1533,.T.);
#3254=EDGE_CURVE('',#2658,#2659,#1534,.T.);
#3255=EDGE_CURVE('',#2658,#2660,#1535,.T.);
#3256=EDGE_CURVE('',#2661,#2659,#1536,.T.);
#3257=EDGE_CURVE('',#2660,#2661,#1537,.T.);
#3258=EDGE_CURVE('',#2660,#2662,#1538,.T.);
#3259=EDGE_CURVE('',#2663,#2661,#1539,.T.);
#3260=EDGE_CURVE('',#2662,#2663,#1540,.T.);
#3261=EDGE_CURVE('',#2662,#2664,#1541,.T.);
#3262=EDGE_CURVE('',#2665,#2663,#1542,.T.);
#3263=EDGE_CURVE('',#2664,#2665,#1543,.T.);
#3264=EDGE_CURVE('',#2664,#2666,#1544,.T.);
#3265=EDGE_CURVE('',#2667,#2665,#1545,.T.);
#3266=EDGE_CURVE('',#2666,#2667,#1546,.T.);
#3267=EDGE_CURVE('',#2666,#2668,#1547,.T.);
#3268=EDGE_CURVE('',#2669,#2667,#1548,.T.);
#3269=EDGE_CURVE('',#2668,#2669,#1549,.T.);
#3270=EDGE_CURVE('',#2668,#2670,#1550,.T.);
#3271=EDGE_CURVE('',#2671,#2669,#1551,.T.);
#3272=EDGE_CURVE('',#2670,#2671,#1552,.T.);
#3273=EDGE_CURVE('',#2670,#2672,#1553,.T.);
#3274=EDGE_CURVE('',#2673,#2671,#1554,.T.);
#3275=EDGE_CURVE('',#2672,#2673,#1555,.T.);
#3276=EDGE_CURVE('',#2672,#2674,#1556,.T.);
#3277=EDGE_CURVE('',#2675,#2673,#1557,.T.);
#3278=EDGE_CURVE('',#2674,#2675,#1558,.T.);
#3279=EDGE_CURVE('',#2674,#2676,#1559,.T.);
#3280=EDGE_CURVE('',#2677,#2675,#1560,.T.);
#3281=EDGE_CURVE('',#2676,#2677,#1561,.T.);
#3282=EDGE_CURVE('',#2676,#2678,#1562,.T.);
#3283=EDGE_CURVE('',#2679,#2677,#1563,.T.);
#3284=EDGE_CURVE('',#2678,#2679,#1564,.T.);
#3285=EDGE_CURVE('',#2678,#2680,#1565,.T.);
#3286=EDGE_CURVE('',#2681,#2679,#1566,.T.);
#3287=EDGE_CURVE('',#2680,#2681,#1567,.T.);
#3288=EDGE_CURVE('',#2680,#2682,#1568,.T.);
#3289=EDGE_CURVE('',#2683,#2681,#1569,.T.);
#3290=EDGE_CURVE('',#2682,#2683,#1570,.T.);
#3291=EDGE_CURVE('',#2682,#2684,#1571,.T.);
#3292=EDGE_CURVE('',#2685,#2683,#1572,.T.);
#3293=EDGE_CURVE('',#2684,#2685,#1573,.T.);
#3294=EDGE_CURVE('',#2684,#2686,#1574,.T.);
#3295=EDGE_CURVE('',#2687,#2685,#1575,.T.);
#3296=EDGE_CURVE('',#2686,#2687,#1576,.T.);
#3297=EDGE_CURVE('',#2686,#2688,#1577,.T.);
#3298=EDGE_CURVE('',#2689,#2687,#1578,.T.);
#3299=EDGE_CURVE('',#2688,#2689,#1579,.T.);
#3300=EDGE_CURVE('',#2688,#2690,#1580,.T.);
#3301=EDGE_CURVE('',#2691,#2689,#1581,.T.);
#3302=EDGE_CURVE('',#2690,#2691,#1582,.T.);
#3303=EDGE_CURVE('',#2690,#2692,#1583,.T.);
#3304=EDGE_CURVE('',#2693,#2691,#1584,.T.);
#3305=EDGE_CURVE('',#2692,#2693,#1585,.T.);
#3306=EDGE_CURVE('',#2692,#2694,#1586,.T.);
#3307=EDGE_CURVE('',#2695,#2693,#1587,.T.);
#3308=EDGE_CURVE('',#2694,#2695,#1588,.T.);
#3309=EDGE_CURVE('',#2694,#2696,#1589,.T.);
#3310=EDGE_CURVE('',#2697,#2695,#1590,.T.);
#3311=EDGE_CURVE('',#2696,#2697,#1591,.T.);
#3312=EDGE_CURVE('',#2696,#2698,#1592,.T.);
#3313=EDGE_CURVE('',#2699,#2697,#1593,.T.);
#3314=EDGE_CURVE('',#2698,#2699,#1594,.T.);
#3315=EDGE_CURVE('',#2698,#2700,#1595,.T.);
#3316=EDGE_CURVE('',#2701,#2699,#1596,.T.);
#3317=EDGE_CURVE('',#2700,#2701,#1597,.T.);
#3318=EDGE_CURVE('',#2700,#2702,#1598,.T.);
#3319=EDGE_CURVE('',#2703,#2701,#1599,.T.);
#3320=EDGE_CURVE('',#2702,#2703,#1600,.T.);
#3321=EDGE_CURVE('',#2702,#2704,#1601,.T.);
#3322=EDGE_CURVE('',#2705,#2703,#1602,.T.);
#3323=EDGE_CURVE('',#2704,#2705,#1603,.T.);
#3324=EDGE_CURVE('',#2704,#2706,#1604,.T.);
#3325=EDGE_CURVE('',#2707,#2705,#1605,.T.);
#3326=EDGE_CURVE('',#2706,#2707,#1606,.T.);
#3327=EDGE_CURVE('',#2706,#2708,#1607,.T.);
#3328=EDGE_CURVE('',#2709,#2707,#1608,.T.);
#3329=EDGE_CURVE('',#2708,#2709,#1609,.T.);
#3330=EDGE_CURVE('',#2708,#2710,#1610,.T.);
#3331=EDGE_CURVE('',#2711,#2709,#1611,.T.);
#3332=EDGE_CURVE('',#2710,#2711,#1612,.T.);
#3333=EDGE_CURVE('',#2710,#2712,#1613,.T.);
#3334=EDGE_CURVE('',#2713,#2711,#1614,.T.);
#3335=EDGE_CURVE('',#2712,#2713,#1615,.T.);
#3336=EDGE_CURVE('',#2712,#2714,#1616,.T.);
#3337=EDGE_CURVE('',#2715,#2713,#1617,.T.);
#3338=EDGE_CURVE('',#2714,#2715,#1618,.T.);
#3339=EDGE_CURVE('',#2714,#2716,#1619,.T.);
#3340=EDGE_CURVE('',#2717,#2715,#1620,.T.);
#3341=EDGE_CURVE('',#2716,#2717,#1621,.T.);
#3342=EDGE_CURVE('',#2716,#2718,#1622,.T.);
#3343=EDGE_CURVE('',#2719,#2717,#1623,.T.);
#3344=EDGE_CURVE('',#2718,#2719,#1624,.T.);
#3345=EDGE_CURVE('',#2718,#2720,#1625,.T.);
#3346=EDGE_CURVE('',#2721,#2719,#1626,.T.);
#3347=EDGE_CURVE('',#2720,#2721,#1627,.T.);
#3348=EDGE_CURVE('',#2720,#2722,#1628,.T.);
#3349=EDGE_CURVE('',#2723,#2721,#1629,.T.);
#3350=EDGE_CURVE('',#2722,#2723,#1630,.T.);
#3351=EDGE_CURVE('',#2722,#2724,#1631,.T.);
#3352=EDGE_CURVE('',#2725,#2723,#1632,.T.);
#3353=EDGE_CURVE('',#2724,#2725,#1633,.T.);
#3354=EDGE_CURVE('',#2724,#2726,#1634,.T.);
#3355=EDGE_CURVE('',#2727,#2725,#1635,.T.);
#3356=EDGE_CURVE('',#2726,#2727,#1636,.T.);
#3357=EDGE_CURVE('',#2726,#2728,#1637,.T.);
#3358=EDGE_CURVE('',#2729,#2727,#1638,.T.);
#3359=EDGE_CURVE('',#2728,#2729,#1639,.T.);
#3360=EDGE_CURVE('',#2728,#2730,#1640,.T.);
#3361=EDGE_CURVE('',#2731,#2729,#1641,.T.);
#3362=EDGE_CURVE('',#2730,#2731,#1642,.T.);
#3363=EDGE_CURVE('',#2730,#2732,#1643,.T.);
#3364=EDGE_CURVE('',#2733,#2731,#1644,.T.);
#3365=EDGE_CURVE('',#2732,#2733,#1645,.T.);
#3366=EDGE_CURVE('',#2732,#2734,#1646,.T.);
#3367=EDGE_CURVE('',#2735,#2733,#1647,.T.);
#3368=EDGE_CURVE('',#2734,#2735,#1648,.T.);
#3369=EDGE_CURVE('',#2734,#2736,#1649,.T.);
#3370=EDGE_CURVE('',#2737,#2735,#1650,.T.);
#3371=EDGE_CURVE('',#2736,#2737,#1651,.T.);
#3372=EDGE_CURVE('',#2736,#2738,#1652,.T.);
#3373=EDGE_CURVE('',#2739,#2737,#1653,.T.);
#3374=EDGE_CURVE('',#2738,#2739,#1654,.T.);
#3375=EDGE_CURVE('',#2738,#2740,#1655,.T.);
#3376=EDGE_CURVE('',#2741,#2739,#1656,.T.);
#3377=EDGE_CURVE('',#2740,#2741,#1657,.T.);
#3378=EDGE_CURVE('',#2740,#2646,#1658,.T.);
#3379=EDGE_CURVE('',#2648,#2741,#1659,.T.);
#3380=EDGE_CURVE('',#2742,#2743,#1660,.T.);
#3381=EDGE_CURVE('',#2742,#2744,#1661,.T.);
#3382=EDGE_CURVE('',#2744,#2745,#1662,.T.);
#3383=EDGE_CURVE('',#2743,#2745,#1663,.T.);
#3384=EDGE_CURVE('',#2746,#2742,#1664,.T.);
#3385=EDGE_CURVE('',#2746,#2747,#1665,.T.);
#3386=EDGE_CURVE('',#2747,#2744,#1666,.T.);
#3387=EDGE_CURVE('',#2748,#2746,#1667,.T.);
#3388=EDGE_CURVE('',#2748,#2749,#1668,.T.);
#3389=EDGE_CURVE('',#2749,#2747,#1669,.T.);
#3390=EDGE_CURVE('',#2750,#2748,#1670,.T.);
#3391=EDGE_CURVE('',#2750,#2751,#1671,.T.);
#3392=EDGE_CURVE('',#2751,#2749,#1672,.T.);
#3393=EDGE_CURVE('',#2752,#2750,#1673,.T.);
#3394=EDGE_CURVE('',#2752,#2753,#1674,.T.);
#3395=EDGE_CURVE('',#2753,#2751,#1675,.T.);
#3396=EDGE_CURVE('',#2743,#2752,#1676,.T.);
#3397=EDGE_CURVE('',#2745,#2753,#1677,.T.);
#3398=EDGE_CURVE('',#2754,#2754,#2321,.T.);
#3399=EDGE_CURVE('',#2755,#2755,#2322,.T.);
#3400=EDGE_CURVE('',#2755,#2754,#1678,.T.);
#3401=EDGE_CURVE('',#2756,#2756,#2323,.F.);
#3402=EDGE_CURVE('',#2756,#2755,#1679,.T.);
#3403=EDGE_CURVE('',#2757,#2757,#2324,.T.);
#3404=EDGE_CURVE('',#2757,#2756,#1680,.T.);
#3405=EDGE_CURVE('',#2758,#2759,#1681,.T.);
#3406=EDGE_CURVE('',#2760,#2758,#2325,.T.);
#3407=EDGE_CURVE('',#2761,#2760,#1682,.T.);
#3408=EDGE_CURVE('',#2759,#2761,#2326,.T.);
#3409=EDGE_CURVE('',#2761,#2762,#1683,.T.);
#3410=EDGE_CURVE('',#2762,#2763,#1684,.T.);
#3411=EDGE_CURVE('',#2763,#2764,#1685,.T.);
#3412=EDGE_CURVE('',#2764,#2765,#1686,.T.);
#3413=EDGE_CURVE('',#2765,#2766,#2327,.T.);
#3414=EDGE_CURVE('',#2766,#2759,#1687,.T.);
#3415=EDGE_CURVE('',#2767,#2767,#2328,.T.);
#3416=EDGE_CURVE('',#2768,#2768,#2329,.T.);
#3417=EDGE_CURVE('',#2768,#2769,#1688,.T.);
#3418=EDGE_CURVE('',#2770,#2769,#2330,.T.);
#3419=EDGE_CURVE('',#2770,#2769,#2331,.T.);
#3420=EDGE_CURVE('',#2770,#2769,#1689,.T.);
#3421=EDGE_CURVE('',#2766,#2771,#2332,.T.);
#3422=EDGE_CURVE('',#2771,#2762,#1690,.T.);
#3423=EDGE_CURVE('',#2772,#2762,#1691,.T.);
#3424=EDGE_CURVE('',#2773,#2772,#1692,.T.);
#3425=EDGE_CURVE('',#2766,#2773,#1693,.T.);
#3426=EDGE_CURVE('',#2772,#2774,#1694,.T.);
#3427=EDGE_CURVE('',#2769,#2774,#1695,.T.);
#3428=EDGE_CURVE('',#2775,#2770,#1696,.T.);
#3429=EDGE_CURVE('',#2773,#2775,#1697,.T.);
#3430=EDGE_CURVE('',#2758,#2775,#1698,.T.);
#3431=EDGE_CURVE('',#2774,#2760,#1699,.T.);
#3432=EDGE_CURVE('',#2776,#2776,#2333,.T.);
#3433=EDGE_CURVE('',#2776,#2767,#1700,.T.);
#3434=EDGE_CURVE('',#2777,#2765,#1701,.T.);
#3435=EDGE_CURVE('',#2777,#2778,#2334,.T.);
#3436=EDGE_CURVE('',#2771,#2778,#1702,.T.);
#3437=EDGE_CURVE('',#2779,#2764,#1703,.T.);
#3438=EDGE_CURVE('',#2777,#2779,#1704,.T.);
#3439=EDGE_CURVE('',#2779,#2780,#1705,.T.);
#3440=EDGE_CURVE('',#2780,#2763,#1706,.T.);
#3441=EDGE_CURVE('',#2780,#2778,#1707,.T.);
#3442=ORIENTED_EDGE('',*,*,#2781,.F.);
#3443=ORIENTED_EDGE('',*,*,#2782,.T.);
#3444=ORIENTED_EDGE('',*,*,#2783,.F.);
#3445=ORIENTED_EDGE('',*,*,#2782,.F.);
#3446=ORIENTED_EDGE('',*,*,#2784,.F.);
#3447=ORIENTED_EDGE('',*,*,#2785,.T.);
#3448=ORIENTED_EDGE('',*,*,#2786,.F.);
#3449=ORIENTED_EDGE('',*,*,#2785,.F.);
#3450=ORIENTED_EDGE('',*,*,#2787,.F.);
#3451=ORIENTED_EDGE('',*,*,#2788,.T.);
#3452=ORIENTED_EDGE('',*,*,#2789,.F.);
#3453=ORIENTED_EDGE('',*,*,#2788,.F.);
#3454=ORIENTED_EDGE('',*,*,#2790,.F.);
#3455=ORIENTED_EDGE('',*,*,#2791,.T.);
#3456=ORIENTED_EDGE('',*,*,#2792,.F.);
#3457=ORIENTED_EDGE('',*,*,#2791,.F.);
#3458=ORIENTED_EDGE('',*,*,#2793,.F.);
#3459=ORIENTED_EDGE('',*,*,#2794,.T.);
#3460=ORIENTED_EDGE('',*,*,#2795,.F.);
#3461=ORIENTED_EDGE('',*,*,#2794,.F.);
#3462=ORIENTED_EDGE('',*,*,#2796,.F.);
#3463=ORIENTED_EDGE('',*,*,#2797,.T.);
#3464=ORIENTED_EDGE('',*,*,#2798,.F.);
#3465=ORIENTED_EDGE('',*,*,#2797,.F.);
#3466=ORIENTED_EDGE('',*,*,#2799,.F.);
#3467=ORIENTED_EDGE('',*,*,#2800,.T.);
#3468=ORIENTED_EDGE('',*,*,#2801,.F.);
#3469=ORIENTED_EDGE('',*,*,#2800,.F.);
#3470=ORIENTED_EDGE('',*,*,#2802,.T.);
#3471=ORIENTED_EDGE('',*,*,#2803,.T.);
#3472=ORIENTED_EDGE('',*,*,#2804,.F.);
#3473=ORIENTED_EDGE('',*,*,#2805,.F.);
#3474=ORIENTED_EDGE('',*,*,#2806,.T.);
#3475=ORIENTED_EDGE('',*,*,#2805,.T.);
#3476=ORIENTED_EDGE('',*,*,#2807,.F.);
#3477=ORIENTED_EDGE('',*,*,#2808,.F.);
#3478=ORIENTED_EDGE('',*,*,#2809,.T.);
#3479=ORIENTED_EDGE('',*,*,#2808,.T.);
#3480=ORIENTED_EDGE('',*,*,#2810,.F.);
#3481=ORIENTED_EDGE('',*,*,#2811,.F.);
#3482=ORIENTED_EDGE('',*,*,#2812,.T.);
#3483=ORIENTED_EDGE('',*,*,#2811,.T.);
#3484=ORIENTED_EDGE('',*,*,#2813,.F.);
#3485=ORIENTED_EDGE('',*,*,#2803,.F.);
#3486=ORIENTED_EDGE('',*,*,#2813,.T.);
#3487=ORIENTED_EDGE('',*,*,#2810,.T.);
#3488=ORIENTED_EDGE('',*,*,#2807,.T.);
#3489=ORIENTED_EDGE('',*,*,#2804,.T.);
#3490=ORIENTED_EDGE('',*,*,#2783,.T.);
#3491=ORIENTED_EDGE('',*,*,#2786,.T.);
#3492=ORIENTED_EDGE('',*,*,#2789,.T.);
#3493=ORIENTED_EDGE('',*,*,#2792,.T.);
#3494=ORIENTED_EDGE('',*,*,#2795,.T.);
#3495=ORIENTED_EDGE('',*,*,#2798,.T.);
#3496=ORIENTED_EDGE('',*,*,#2801,.T.);
#3497=ORIENTED_EDGE('',*,*,#2812,.F.);
#3498=ORIENTED_EDGE('',*,*,#2802,.F.);
#3499=ORIENTED_EDGE('',*,*,#2806,.F.);
#3500=ORIENTED_EDGE('',*,*,#2809,.F.);
#3501=ORIENTED_EDGE('',*,*,#2781,.T.);
#3502=ORIENTED_EDGE('',*,*,#2784,.T.);
#3503=ORIENTED_EDGE('',*,*,#2787,.T.);
#3504=ORIENTED_EDGE('',*,*,#2790,.T.);
#3505=ORIENTED_EDGE('',*,*,#2793,.T.);
#3506=ORIENTED_EDGE('',*,*,#2796,.T.);
#3507=ORIENTED_EDGE('',*,*,#2799,.T.);
#3508=ORIENTED_EDGE('',*,*,#2814,.F.);
#3509=ORIENTED_EDGE('',*,*,#2815,.T.);
#3510=ORIENTED_EDGE('',*,*,#2816,.F.);
#3511=ORIENTED_EDGE('',*,*,#2815,.F.);
#3512=ORIENTED_EDGE('',*,*,#2817,.F.);
#3513=ORIENTED_EDGE('',*,*,#2818,.T.);
#3514=ORIENTED_EDGE('',*,*,#2819,.F.);
#3515=ORIENTED_EDGE('',*,*,#2818,.F.);
#3516=ORIENTED_EDGE('',*,*,#2820,.F.);
#3517=ORIENTED_EDGE('',*,*,#2821,.T.);
#3518=ORIENTED_EDGE('',*,*,#2822,.T.);
#3519=ORIENTED_EDGE('',*,*,#2821,.F.);
#3520=ORIENTED_EDGE('',*,*,#2822,.F.);
#3521=ORIENTED_EDGE('',*,*,#2823,.F.);
#3522=ORIENTED_EDGE('',*,*,#2823,.T.);
#3523=ORIENTED_EDGE('',*,*,#2824,.T.);
#3524=ORIENTED_EDGE('',*,*,#2825,.F.);
#3525=ORIENTED_EDGE('',*,*,#2824,.F.);
#3526=ORIENTED_EDGE('',*,*,#2826,.F.);
#3527=ORIENTED_EDGE('',*,*,#2827,.T.);
#3528=ORIENTED_EDGE('',*,*,#2828,.F.);
#3529=ORIENTED_EDGE('',*,*,#2827,.F.);
#3530=ORIENTED_EDGE('',*,*,#2826,.T.);
#3531=ORIENTED_EDGE('',*,*,#2825,.T.);
#3532=ORIENTED_EDGE('',*,*,#2829,.T.);
#3533=ORIENTED_EDGE('',*,*,#2830,.T.);
#3534=ORIENTED_EDGE('',*,*,#2831,.F.);
#3535=ORIENTED_EDGE('',*,*,#2832,.F.);
#3536=ORIENTED_EDGE('',*,*,#2833,.T.);
#3537=ORIENTED_EDGE('',*,*,#2832,.T.);
#3538=ORIENTED_EDGE('',*,*,#2834,.F.);
#3539=ORIENTED_EDGE('',*,*,#2835,.F.);
#3540=ORIENTED_EDGE('',*,*,#2836,.T.);
#3541=ORIENTED_EDGE('',*,*,#2835,.T.);
#3542=ORIENTED_EDGE('',*,*,#2837,.F.);
#3543=ORIENTED_EDGE('',*,*,#2838,.F.);
#3544=ORIENTED_EDGE('',*,*,#2839,.T.);
#3545=ORIENTED_EDGE('',*,*,#2838,.T.);
#3546=ORIENTED_EDGE('',*,*,#2840,.F.);
#3547=ORIENTED_EDGE('',*,*,#2830,.F.);
#3548=ORIENTED_EDGE('',*,*,#2840,.T.);
#3549=ORIENTED_EDGE('',*,*,#2837,.T.);
#3550=ORIENTED_EDGE('',*,*,#2834,.T.);
#3551=ORIENTED_EDGE('',*,*,#2831,.T.);
#3552=ORIENTED_EDGE('',*,*,#2816,.T.);
#3553=ORIENTED_EDGE('',*,*,#2819,.T.);
#3554=ORIENTED_EDGE('',*,*,#2828,.T.);
#3555=ORIENTED_EDGE('',*,*,#2839,.F.);
#3556=ORIENTED_EDGE('',*,*,#2829,.F.);
#3557=ORIENTED_EDGE('',*,*,#2833,.F.);
#3558=ORIENTED_EDGE('',*,*,#2836,.F.);
#3559=ORIENTED_EDGE('',*,*,#2814,.T.);
#3560=ORIENTED_EDGE('',*,*,#2817,.T.);
#3561=ORIENTED_EDGE('',*,*,#2820,.T.);
#3562=ORIENTED_EDGE('',*,*,#2841,.F.);
#3563=ORIENTED_EDGE('',*,*,#2842,.T.);
#3564=ORIENTED_EDGE('',*,*,#2843,.F.);
#3565=ORIENTED_EDGE('',*,*,#2842,.F.);
#3566=ORIENTED_EDGE('',*,*,#2841,.T.);
#3567=ORIENTED_EDGE('',*,*,#2844,.T.);
#3568=ORIENTED_EDGE('',*,*,#2845,.F.);
#3569=ORIENTED_EDGE('',*,*,#2844,.F.);
#3570=ORIENTED_EDGE('',*,*,#2846,.T.);
#3571=ORIENTED_EDGE('',*,*,#2847,.T.);
#3572=ORIENTED_EDGE('',*,*,#2846,.F.);
#3573=ORIENTED_EDGE('',*,*,#2847,.F.);
#3574=ORIENTED_EDGE('',*,*,#2848,.F.);
#3575=ORIENTED_EDGE('',*,*,#2849,.T.);
#3576=ORIENTED_EDGE('',*,*,#2845,.T.);
#3577=ORIENTED_EDGE('',*,*,#2849,.F.);
#3578=ORIENTED_EDGE('',*,*,#2848,.T.);
#3579=ORIENTED_EDGE('',*,*,#2843,.T.);
#3580=ORIENTED_EDGE('',*,*,#2850,.F.);
#3581=ORIENTED_EDGE('',*,*,#2851,.T.);
#3582=ORIENTED_EDGE('',*,*,#2852,.T.);
#3583=ORIENTED_EDGE('',*,*,#2851,.F.);
#3584=ORIENTED_EDGE('',*,*,#2853,.F.);
#3585=ORIENTED_EDGE('',*,*,#2854,.T.);
#3586=ORIENTED_EDGE('',*,*,#2855,.T.);
#3587=ORIENTED_EDGE('',*,*,#2854,.F.);
#3588=ORIENTED_EDGE('',*,*,#2853,.T.);
#3589=ORIENTED_EDGE('',*,*,#2850,.T.);
#3590=ORIENTED_EDGE('',*,*,#2855,.F.);
#3591=ORIENTED_EDGE('',*,*,#2852,.F.);
#3592=ORIENTED_EDGE('',*,*,#2856,.F.);
#3593=ORIENTED_EDGE('',*,*,#2857,.T.);
#3594=ORIENTED_EDGE('',*,*,#2858,.T.);
#3595=ORIENTED_EDGE('',*,*,#2857,.F.);
#3596=ORIENTED_EDGE('',*,*,#2859,.F.);
#3597=ORIENTED_EDGE('',*,*,#2860,.T.);
#3598=ORIENTED_EDGE('',*,*,#2861,.T.);
#3599=ORIENTED_EDGE('',*,*,#2860,.F.);
#3600=ORIENTED_EDGE('',*,*,#2859,.T.);
#3601=ORIENTED_EDGE('',*,*,#2856,.T.);
#3602=ORIENTED_EDGE('',*,*,#2861,.F.);
#3603=ORIENTED_EDGE('',*,*,#2858,.F.);
#3604=ORIENTED_EDGE('',*,*,#2862,.F.);
#3605=ORIENTED_EDGE('',*,*,#2863,.T.);
#3606=ORIENTED_EDGE('',*,*,#2864,.T.);
#3607=ORIENTED_EDGE('',*,*,#2863,.F.);
#3608=ORIENTED_EDGE('',*,*,#2865,.F.);
#3609=ORIENTED_EDGE('',*,*,#2866,.T.);
#3610=ORIENTED_EDGE('',*,*,#2867,.T.);
#3611=ORIENTED_EDGE('',*,*,#2866,.F.);
#3612=ORIENTED_EDGE('',*,*,#2865,.T.);
#3613=ORIENTED_EDGE('',*,*,#2862,.T.);
#3614=ORIENTED_EDGE('',*,*,#2867,.F.);
#3615=ORIENTED_EDGE('',*,*,#2864,.F.);
#3616=ORIENTED_EDGE('',*,*,#2868,.F.);
#3617=ORIENTED_EDGE('',*,*,#2869,.T.);
#3618=ORIENTED_EDGE('',*,*,#2870,.T.);
#3619=ORIENTED_EDGE('',*,*,#2869,.F.);
#3620=ORIENTED_EDGE('',*,*,#2870,.F.);
#3621=ORIENTED_EDGE('',*,*,#2871,.F.);
#3622=ORIENTED_EDGE('',*,*,#2872,.T.);
#3623=ORIENTED_EDGE('',*,*,#2873,.F.);
#3624=ORIENTED_EDGE('',*,*,#2874,.F.);
#3625=ORIENTED_EDGE('',*,*,#2872,.F.);
#3626=ORIENTED_EDGE('',*,*,#2871,.T.);
#3627=ORIENTED_EDGE('',*,*,#2875,.T.);
#3628=ORIENTED_EDGE('',*,*,#2876,.T.);
#3629=ORIENTED_EDGE('',*,*,#2873,.T.);
#3630=ORIENTED_EDGE('',*,*,#2874,.T.);
#3631=ORIENTED_EDGE('',*,*,#2877,.T.);
#3632=ORIENTED_EDGE('',*,*,#2878,.T.);
#3633=ORIENTED_EDGE('',*,*,#2879,.T.);
#3634=ORIENTED_EDGE('',*,*,#2880,.F.);
#3635=ORIENTED_EDGE('',*,*,#2881,.F.);
#3636=ORIENTED_EDGE('',*,*,#2882,.F.);
#3637=ORIENTED_EDGE('',*,*,#2883,.T.);
#3638=ORIENTED_EDGE('',*,*,#2884,.T.);
#3639=ORIENTED_EDGE('',*,*,#2885,.F.);
#3640=ORIENTED_EDGE('',*,*,#2886,.F.);
#3641=ORIENTED_EDGE('',*,*,#2881,.T.);
#3642=ORIENTED_EDGE('',*,*,#2887,.T.);
#3643=ORIENTED_EDGE('',*,*,#2879,.F.);
#3644=ORIENTED_EDGE('',*,*,#2888,.F.);
#3645=ORIENTED_EDGE('',*,*,#2885,.T.);
#3646=ORIENTED_EDGE('',*,*,#2882,.T.);
#3647=ORIENTED_EDGE('',*,*,#2888,.T.);
#3648=ORIENTED_EDGE('',*,*,#2878,.F.);
#3649=ORIENTED_EDGE('',*,*,#2889,.F.);
#3650=ORIENTED_EDGE('',*,*,#2886,.T.);
#3651=ORIENTED_EDGE('',*,*,#2889,.T.);
#3652=ORIENTED_EDGE('',*,*,#2877,.F.);
#3653=ORIENTED_EDGE('',*,*,#2876,.F.);
#3654=ORIENTED_EDGE('',*,*,#2890,.F.);
#3655=ORIENTED_EDGE('',*,*,#2880,.T.);
#3656=ORIENTED_EDGE('',*,*,#2890,.T.);
#3657=ORIENTED_EDGE('',*,*,#2875,.F.);
#3658=ORIENTED_EDGE('',*,*,#2887,.F.);
#3659=ORIENTED_EDGE('',*,*,#2883,.F.);
#3660=ORIENTED_EDGE('',*,*,#2884,.F.);
#3661=ORIENTED_EDGE('',*,*,#2891,.T.);
#3662=ORIENTED_EDGE('',*,*,#2892,.T.);
#3663=ORIENTED_EDGE('',*,*,#2891,.F.);
#3664=ORIENTED_EDGE('',*,*,#2892,.F.);
#3665=ORIENTED_EDGE('',*,*,#2868,.T.);
#3666=ORIENTED_EDGE('',*,*,#2893,.F.);
#3667=ORIENTED_EDGE('',*,*,#2894,.F.);
#3668=ORIENTED_EDGE('',*,*,#2895,.T.);
#3669=ORIENTED_EDGE('',*,*,#2896,.F.);
#3670=ORIENTED_EDGE('',*,*,#2897,.F.);
#3671=ORIENTED_EDGE('',*,*,#2895,.F.);
#3672=ORIENTED_EDGE('',*,*,#2898,.F.);
#3673=ORIENTED_EDGE('',*,*,#2899,.T.);
#3674=ORIENTED_EDGE('',*,*,#2900,.F.);
#3675=ORIENTED_EDGE('',*,*,#2899,.F.);
#3676=ORIENTED_EDGE('',*,*,#2898,.T.);
#3677=ORIENTED_EDGE('',*,*,#2901,.F.);
#3678=ORIENTED_EDGE('',*,*,#2902,.T.);
#3679=ORIENTED_EDGE('',*,*,#2903,.F.);
#3680=ORIENTED_EDGE('',*,*,#2902,.F.);
#3681=ORIENTED_EDGE('',*,*,#2901,.T.);
#3682=ORIENTED_EDGE('',*,*,#2904,.F.);
#3683=ORIENTED_EDGE('',*,*,#2905,.T.);
#3684=ORIENTED_EDGE('',*,*,#2906,.F.);
#3685=ORIENTED_EDGE('',*,*,#2905,.F.);
#3686=ORIENTED_EDGE('',*,*,#2904,.T.);
#3687=ORIENTED_EDGE('',*,*,#2907,.F.);
#3688=ORIENTED_EDGE('',*,*,#2908,.T.);
#3689=ORIENTED_EDGE('',*,*,#2909,.F.);
#3690=ORIENTED_EDGE('',*,*,#2908,.F.);
#3691=ORIENTED_EDGE('',*,*,#2907,.T.);
#3692=ORIENTED_EDGE('',*,*,#2910,.F.);
#3693=ORIENTED_EDGE('',*,*,#2911,.F.);
#3694=ORIENTED_EDGE('',*,*,#2912,.F.);
#3695=ORIENTED_EDGE('',*,*,#2913,.F.);
#3696=ORIENTED_EDGE('',*,*,#2914,.F.);
#3697=ORIENTED_EDGE('',*,*,#2911,.T.);
#3698=ORIENTED_EDGE('',*,*,#2915,.F.);
#3699=ORIENTED_EDGE('',*,*,#2916,.T.);
#3700=ORIENTED_EDGE('',*,*,#2917,.F.);
#3701=ORIENTED_EDGE('',*,*,#2918,.F.);
#3702=ORIENTED_EDGE('',*,*,#2919,.F.);
#3703=ORIENTED_EDGE('',*,*,#2916,.F.);
#3704=ORIENTED_EDGE('',*,*,#2920,.F.);
#3705=ORIENTED_EDGE('',*,*,#2921,.T.);
#3706=ORIENTED_EDGE('',*,*,#2922,.F.);
#3707=ORIENTED_EDGE('',*,*,#2923,.F.);
#3708=ORIENTED_EDGE('',*,*,#2924,.F.);
#3709=ORIENTED_EDGE('',*,*,#2921,.F.);
#3710=ORIENTED_EDGE('',*,*,#2925,.F.);
#3711=ORIENTED_EDGE('',*,*,#2926,.T.);
#3712=ORIENTED_EDGE('',*,*,#2927,.F.);
#3713=ORIENTED_EDGE('',*,*,#2928,.F.);
#3714=ORIENTED_EDGE('',*,*,#2929,.F.);
#3715=ORIENTED_EDGE('',*,*,#2926,.F.);
#3716=ORIENTED_EDGE('',*,*,#2930,.F.);
#3717=ORIENTED_EDGE('',*,*,#2931,.T.);
#3718=ORIENTED_EDGE('',*,*,#2932,.T.);
#3719=ORIENTED_EDGE('',*,*,#2912,.T.);
#3720=ORIENTED_EDGE('',*,*,#2910,.T.);
#3721=ORIENTED_EDGE('',*,*,#2914,.T.);
#3722=ORIENTED_EDGE('',*,*,#2933,.T.);
#3723=ORIENTED_EDGE('',*,*,#2927,.T.);
#3724=ORIENTED_EDGE('',*,*,#2929,.T.);
#3725=ORIENTED_EDGE('',*,*,#2925,.T.);
#3726=ORIENTED_EDGE('',*,*,#2934,.T.);
#3727=ORIENTED_EDGE('',*,*,#2922,.T.);
#3728=ORIENTED_EDGE('',*,*,#2924,.T.);
#3729=ORIENTED_EDGE('',*,*,#2920,.T.);
#3730=ORIENTED_EDGE('',*,*,#2935,.T.);
#3731=ORIENTED_EDGE('',*,*,#2917,.T.);
#3732=ORIENTED_EDGE('',*,*,#2919,.T.);
#3733=ORIENTED_EDGE('',*,*,#2915,.T.);
#3734=ORIENTED_EDGE('',*,*,#2936,.T.);
#3735=ORIENTED_EDGE('',*,*,#2931,.F.);
#3736=ORIENTED_EDGE('',*,*,#2937,.T.);
#3737=ORIENTED_EDGE('',*,*,#2936,.F.);
#3738=ORIENTED_EDGE('',*,*,#2918,.T.);
#3739=ORIENTED_EDGE('',*,*,#2935,.F.);
#3740=ORIENTED_EDGE('',*,*,#2923,.T.);
#3741=ORIENTED_EDGE('',*,*,#2934,.F.);
#3742=ORIENTED_EDGE('',*,*,#2928,.T.);
#3743=ORIENTED_EDGE('',*,*,#2933,.F.);
#3744=ORIENTED_EDGE('',*,*,#2913,.T.);
#3745=ORIENTED_EDGE('',*,*,#2932,.F.);
#3746=ORIENTED_EDGE('',*,*,#2938,.T.);
#3747=ORIENTED_EDGE('',*,*,#2939,.T.);
#3748=ORIENTED_EDGE('',*,*,#2940,.T.);
#3749=ORIENTED_EDGE('',*,*,#2941,.T.);
#3750=ORIENTED_EDGE('',*,*,#2942,.F.);
#3751=ORIENTED_EDGE('',*,*,#2943,.T.);
#3752=ORIENTED_EDGE('',*,*,#2938,.F.);
#3753=ORIENTED_EDGE('',*,*,#2943,.F.);
#3754=ORIENTED_EDGE('',*,*,#2944,.F.);
#3755=ORIENTED_EDGE('',*,*,#2945,.T.);
#3756=ORIENTED_EDGE('',*,*,#2941,.F.);
#3757=ORIENTED_EDGE('',*,*,#2945,.F.);
#3758=ORIENTED_EDGE('',*,*,#2946,.F.);
#3759=ORIENTED_EDGE('',*,*,#2947,.T.);
#3760=ORIENTED_EDGE('',*,*,#2939,.F.);
#3761=ORIENTED_EDGE('',*,*,#2947,.F.);
#3762=ORIENTED_EDGE('',*,*,#2948,.F.);
#3763=ORIENTED_EDGE('',*,*,#2949,.T.);
#3764=ORIENTED_EDGE('',*,*,#2940,.F.);
#3765=ORIENTED_EDGE('',*,*,#2949,.F.);
#3766=ORIENTED_EDGE('',*,*,#2950,.F.);
#3767=ORIENTED_EDGE('',*,*,#2951,.T.);
#3768=ORIENTED_EDGE('',*,*,#2952,.F.);
#3769=ORIENTED_EDGE('',*,*,#2951,.F.);
#3770=ORIENTED_EDGE('',*,*,#2950,.T.);
#3771=ORIENTED_EDGE('',*,*,#2953,.F.);
#3772=ORIENTED_EDGE('',*,*,#2937,.F.);
#3773=ORIENTED_EDGE('',*,*,#2954,.T.);
#3774=ORIENTED_EDGE('',*,*,#2955,.T.);
#3775=ORIENTED_EDGE('',*,*,#2954,.F.);
#3776=ORIENTED_EDGE('',*,*,#2896,.T.);
#3777=ORIENTED_EDGE('',*,*,#2897,.T.);
#3778=ORIENTED_EDGE('',*,*,#2953,.T.);
#3779=ORIENTED_EDGE('',*,*,#2956,.T.);
#3780=ORIENTED_EDGE('',*,*,#2957,.T.);
#3781=ORIENTED_EDGE('',*,*,#2956,.F.);
#3782=ORIENTED_EDGE('',*,*,#2893,.T.);
#3783=ORIENTED_EDGE('',*,*,#2894,.T.);
#3784=ORIENTED_EDGE('',*,*,#2930,.T.);
#3785=ORIENTED_EDGE('',*,*,#2952,.T.);
#3786=ORIENTED_EDGE('',*,*,#2909,.T.);
#3787=ORIENTED_EDGE('',*,*,#2906,.T.);
#3788=ORIENTED_EDGE('',*,*,#2903,.T.);
#3789=ORIENTED_EDGE('',*,*,#2900,.T.);
#3790=ORIENTED_EDGE('',*,*,#2955,.F.);
#3791=ORIENTED_EDGE('',*,*,#2957,.F.);
#3792=ORIENTED_EDGE('',*,*,#2948,.T.);
#3793=ORIENTED_EDGE('',*,*,#2946,.T.);
#3794=ORIENTED_EDGE('',*,*,#2944,.T.);
#3795=ORIENTED_EDGE('',*,*,#2942,.T.);
#3796=ORIENTED_EDGE('',*,*,#2958,.F.);
#3797=ORIENTED_EDGE('',*,*,#2959,.T.);
#3798=ORIENTED_EDGE('',*,*,#2960,.F.);
#3799=ORIENTED_EDGE('',*,*,#2959,.F.);
#3800=ORIENTED_EDGE('',*,*,#2958,.T.);
#3801=ORIENTED_EDGE('',*,*,#2961,.F.);
#3802=ORIENTED_EDGE('',*,*,#2962,.F.);
#3803=ORIENTED_EDGE('',*,*,#2963,.T.);
#3804=ORIENTED_EDGE('',*,*,#2964,.F.);
#3805=ORIENTED_EDGE('',*,*,#2963,.F.);
#3806=ORIENTED_EDGE('',*,*,#2962,.T.);
#3807=ORIENTED_EDGE('',*,*,#2965,.F.);
#3808=ORIENTED_EDGE('',*,*,#2966,.F.);
#3809=ORIENTED_EDGE('',*,*,#2967,.T.);
#3810=ORIENTED_EDGE('',*,*,#2968,.F.);
#3811=ORIENTED_EDGE('',*,*,#2967,.F.);
#3812=ORIENTED_EDGE('',*,*,#2966,.T.);
#3813=ORIENTED_EDGE('',*,*,#2969,.F.);
#3814=ORIENTED_EDGE('',*,*,#2970,.F.);
#3815=ORIENTED_EDGE('',*,*,#2971,.T.);
#3816=ORIENTED_EDGE('',*,*,#2972,.F.);
#3817=ORIENTED_EDGE('',*,*,#2971,.F.);
#3818=ORIENTED_EDGE('',*,*,#2970,.T.);
#3819=ORIENTED_EDGE('',*,*,#2973,.F.);
#3820=ORIENTED_EDGE('',*,*,#2974,.F.);
#3821=ORIENTED_EDGE('',*,*,#2975,.T.);
#3822=ORIENTED_EDGE('',*,*,#2961,.T.);
#3823=ORIENTED_EDGE('',*,*,#2975,.F.);
#3824=ORIENTED_EDGE('',*,*,#2976,.F.);
#3825=ORIENTED_EDGE('',*,*,#2977,.T.);
#3826=ORIENTED_EDGE('',*,*,#2965,.T.);
#3827=ORIENTED_EDGE('',*,*,#2977,.F.);
#3828=ORIENTED_EDGE('',*,*,#2978,.F.);
#3829=ORIENTED_EDGE('',*,*,#2979,.T.);
#3830=ORIENTED_EDGE('',*,*,#2969,.T.);
#3831=ORIENTED_EDGE('',*,*,#2979,.F.);
#3832=ORIENTED_EDGE('',*,*,#2980,.F.);
#3833=ORIENTED_EDGE('',*,*,#2981,.T.);
#3834=ORIENTED_EDGE('',*,*,#2973,.T.);
#3835=ORIENTED_EDGE('',*,*,#2981,.F.);
#3836=ORIENTED_EDGE('',*,*,#2982,.F.);
#3837=ORIENTED_EDGE('',*,*,#2983,.T.);
#3838=ORIENTED_EDGE('',*,*,#2984,.T.);
#3839=ORIENTED_EDGE('',*,*,#2983,.F.);
#3840=ORIENTED_EDGE('',*,*,#2984,.F.);
#3841=ORIENTED_EDGE('',*,*,#2985,.F.);
#3842=ORIENTED_EDGE('',*,*,#2986,.F.);
#3843=ORIENTED_EDGE('',*,*,#2987,.T.);
#3844=ORIENTED_EDGE('',*,*,#2985,.T.);
#3845=ORIENTED_EDGE('',*,*,#2987,.F.);
#3846=ORIENTED_EDGE('',*,*,#2988,.F.);
#3847=ORIENTED_EDGE('',*,*,#2989,.T.);
#3848=ORIENTED_EDGE('',*,*,#2990,.T.);
#3849=ORIENTED_EDGE('',*,*,#2989,.F.);
#3850=ORIENTED_EDGE('',*,*,#2988,.T.);
#3851=ORIENTED_EDGE('',*,*,#2986,.T.);
#3852=ORIENTED_EDGE('',*,*,#2972,.T.);
#3853=ORIENTED_EDGE('',*,*,#2968,.T.);
#3854=ORIENTED_EDGE('',*,*,#2964,.T.);
#3855=ORIENTED_EDGE('',*,*,#2960,.T.);
#3856=ORIENTED_EDGE('',*,*,#2990,.F.);
#3857=ORIENTED_EDGE('',*,*,#2982,.T.);
#3858=ORIENTED_EDGE('',*,*,#2980,.T.);
#3859=ORIENTED_EDGE('',*,*,#2978,.T.);
#3860=ORIENTED_EDGE('',*,*,#2976,.T.);
#3861=ORIENTED_EDGE('',*,*,#2974,.T.);
#3862=ORIENTED_EDGE('',*,*,#2991,.F.);
#3863=ORIENTED_EDGE('',*,*,#2992,.F.);
#3864=ORIENTED_EDGE('',*,*,#2993,.T.);
#3865=ORIENTED_EDGE('',*,*,#2994,.F.);
#3866=ORIENTED_EDGE('',*,*,#2995,.F.);
#3867=ORIENTED_EDGE('',*,*,#2993,.F.);
#3868=ORIENTED_EDGE('',*,*,#2994,.T.);
#3869=ORIENTED_EDGE('',*,*,#2995,.T.);
#3870=ORIENTED_EDGE('',*,*,#2996,.T.);
#3871=ORIENTED_EDGE('',*,*,#2997,.T.);
#3872=ORIENTED_EDGE('',*,*,#2996,.F.);
#3873=ORIENTED_EDGE('',*,*,#2998,.T.);
#3874=ORIENTED_EDGE('',*,*,#2999,.T.);
#3875=ORIENTED_EDGE('',*,*,#3000,.F.);
#3876=ORIENTED_EDGE('',*,*,#2999,.F.);
#3877=ORIENTED_EDGE('',*,*,#3000,.T.);
#3878=ORIENTED_EDGE('',*,*,#3001,.T.);
#3879=ORIENTED_EDGE('',*,*,#3002,.F.);
#3880=ORIENTED_EDGE('',*,*,#3001,.F.);
#3881=ORIENTED_EDGE('',*,*,#2997,.F.);
#3882=ORIENTED_EDGE('',*,*,#3002,.T.);
#3883=ORIENTED_EDGE('',*,*,#3003,.F.);
#3884=ORIENTED_EDGE('',*,*,#3004,.T.);
#3885=ORIENTED_EDGE('',*,*,#2991,.T.);
#3886=ORIENTED_EDGE('',*,*,#2992,.T.);
#3887=ORIENTED_EDGE('',*,*,#3004,.F.);
#3888=ORIENTED_EDGE('',*,*,#3003,.T.);
#3889=ORIENTED_EDGE('',*,*,#3005,.F.);
#3890=ORIENTED_EDGE('',*,*,#3005,.T.);
#3891=ORIENTED_EDGE('',*,*,#3006,.T.);
#3892=ORIENTED_EDGE('',*,*,#2998,.F.);
#3893=ORIENTED_EDGE('',*,*,#3006,.F.);
#3894=ORIENTED_EDGE('',*,*,#3007,.F.);
#3895=ORIENTED_EDGE('',*,*,#3008,.F.);
#3896=ORIENTED_EDGE('',*,*,#3009,.T.);
#3897=ORIENTED_EDGE('',*,*,#3010,.F.);
#3898=ORIENTED_EDGE('',*,*,#3011,.F.);
#3899=ORIENTED_EDGE('',*,*,#3009,.F.);
#3900=ORIENTED_EDGE('',*,*,#3012,.T.);
#3901=ORIENTED_EDGE('',*,*,#3013,.T.);
#3902=ORIENTED_EDGE('',*,*,#3010,.T.);
#3903=ORIENTED_EDGE('',*,*,#3011,.T.);
#3904=ORIENTED_EDGE('',*,*,#3013,.F.);
#3905=ORIENTED_EDGE('',*,*,#3014,.F.);
#3906=ORIENTED_EDGE('',*,*,#3015,.T.);
#3907=ORIENTED_EDGE('',*,*,#3016,.F.);
#3908=ORIENTED_EDGE('',*,*,#3017,.T.);
#3909=ORIENTED_EDGE('',*,*,#3014,.T.);
#3910=ORIENTED_EDGE('',*,*,#3017,.F.);
#3911=ORIENTED_EDGE('',*,*,#3018,.F.);
#3912=ORIENTED_EDGE('',*,*,#3019,.T.);
#3913=ORIENTED_EDGE('',*,*,#3016,.T.);
#3914=ORIENTED_EDGE('',*,*,#3019,.F.);
#3915=ORIENTED_EDGE('',*,*,#3020,.F.);
#3916=ORIENTED_EDGE('',*,*,#3021,.T.);
#3917=ORIENTED_EDGE('',*,*,#3018,.T.);
#3918=ORIENTED_EDGE('',*,*,#3021,.F.);
#3919=ORIENTED_EDGE('',*,*,#3020,.T.);
#3920=ORIENTED_EDGE('',*,*,#3012,.F.);
#3921=ORIENTED_EDGE('',*,*,#3007,.T.);
#3922=ORIENTED_EDGE('',*,*,#3008,.T.);
#3923=ORIENTED_EDGE('',*,*,#3022,.T.);
#3924=ORIENTED_EDGE('',*,*,#3015,.F.);
#3925=ORIENTED_EDGE('',*,*,#3022,.F.);
#3926=ORIENTED_EDGE('',*,*,#3023,.T.);
#3927=ORIENTED_EDGE('',*,*,#3023,.F.);
#3928=ORIENTED_EDGE('',*,*,#3024,.T.);
#3929=ORIENTED_EDGE('',*,*,#3024,.F.);
#3930=ORIENTED_EDGE('',*,*,#3025,.T.);
#3931=ORIENTED_EDGE('',*,*,#3025,.F.);
#3932=ORIENTED_EDGE('',*,*,#3026,.T.);
#3933=ORIENTED_EDGE('',*,*,#3026,.F.);
#3934=ORIENTED_EDGE('',*,*,#3027,.T.);
#3935=ORIENTED_EDGE('',*,*,#3027,.F.);
#3936=ORIENTED_EDGE('',*,*,#3028,.T.);
#3937=ORIENTED_EDGE('',*,*,#3028,.F.);
#3938=ORIENTED_EDGE('',*,*,#3029,.T.);
#3939=ORIENTED_EDGE('',*,*,#3029,.F.);
#3940=ORIENTED_EDGE('',*,*,#3030,.T.);
#3941=ORIENTED_EDGE('',*,*,#3030,.F.);
#3942=ORIENTED_EDGE('',*,*,#3031,.F.);
#3943=ORIENTED_EDGE('',*,*,#3032,.F.);
#3944=ORIENTED_EDGE('',*,*,#3033,.F.);
#3945=ORIENTED_EDGE('',*,*,#3034,.F.);
#3946=ORIENTED_EDGE('',*,*,#3033,.T.);
#3947=ORIENTED_EDGE('',*,*,#3035,.F.);
#3948=ORIENTED_EDGE('',*,*,#3036,.T.);
#3949=ORIENTED_EDGE('',*,*,#3037,.F.);
#3950=ORIENTED_EDGE('',*,*,#3038,.T.);
#3951=ORIENTED_EDGE('',*,*,#3039,.F.);
#3952=ORIENTED_EDGE('',*,*,#3040,.T.);
#3953=ORIENTED_EDGE('',*,*,#3041,.T.);
#3954=ORIENTED_EDGE('',*,*,#3042,.F.);
#3955=ORIENTED_EDGE('',*,*,#3041,.F.);
#3956=ORIENTED_EDGE('',*,*,#3043,.T.);
#3957=ORIENTED_EDGE('',*,*,#3044,.F.);
#3958=ORIENTED_EDGE('',*,*,#3045,.T.);
#3959=ORIENTED_EDGE('',*,*,#3046,.F.);
#3960=ORIENTED_EDGE('',*,*,#3047,.T.);
#3961=ORIENTED_EDGE('',*,*,#3048,.F.);
#3962=ORIENTED_EDGE('',*,*,#3049,.T.);
#3963=ORIENTED_EDGE('',*,*,#3050,.F.);
#3964=ORIENTED_EDGE('',*,*,#3051,.T.);
#3965=ORIENTED_EDGE('',*,*,#3052,.F.);
#3966=ORIENTED_EDGE('',*,*,#3032,.T.);
#3967=ORIENTED_EDGE('',*,*,#3053,.T.);
#3968=ORIENTED_EDGE('',*,*,#3054,.T.);
#3969=ORIENTED_EDGE('',*,*,#3035,.T.);
#3970=ORIENTED_EDGE('',*,*,#3055,.F.);
#3971=ORIENTED_EDGE('',*,*,#3056,.F.);
#3972=ORIENTED_EDGE('',*,*,#3036,.F.);
#3973=ORIENTED_EDGE('',*,*,#3054,.F.);
#3974=ORIENTED_EDGE('',*,*,#3056,.T.);
#3975=ORIENTED_EDGE('',*,*,#3057,.T.);
#3976=ORIENTED_EDGE('',*,*,#3058,.T.);
#3977=ORIENTED_EDGE('',*,*,#3037,.T.);
#3978=ORIENTED_EDGE('',*,*,#3059,.F.);
#3979=ORIENTED_EDGE('',*,*,#3060,.F.);
#3980=ORIENTED_EDGE('',*,*,#3038,.F.);
#3981=ORIENTED_EDGE('',*,*,#3058,.F.);
#3982=ORIENTED_EDGE('',*,*,#3060,.T.);
#3983=ORIENTED_EDGE('',*,*,#3061,.T.);
#3984=ORIENTED_EDGE('',*,*,#3062,.T.);
#3985=ORIENTED_EDGE('',*,*,#3039,.T.);
#3986=ORIENTED_EDGE('',*,*,#3063,.F.);
#3987=ORIENTED_EDGE('',*,*,#3064,.F.);
#3988=ORIENTED_EDGE('',*,*,#3043,.F.);
#3989=ORIENTED_EDGE('',*,*,#3040,.F.);
#3990=ORIENTED_EDGE('',*,*,#3062,.F.);
#3991=ORIENTED_EDGE('',*,*,#3065,.F.);
#3992=ORIENTED_EDGE('',*,*,#3064,.T.);
#3993=ORIENTED_EDGE('',*,*,#3066,.T.);
#3994=ORIENTED_EDGE('',*,*,#3067,.T.);
#3995=ORIENTED_EDGE('',*,*,#3044,.T.);
#3996=ORIENTED_EDGE('',*,*,#3068,.F.);
#3997=ORIENTED_EDGE('',*,*,#3069,.F.);
#3998=ORIENTED_EDGE('',*,*,#3045,.F.);
#3999=ORIENTED_EDGE('',*,*,#3067,.F.);
#4000=ORIENTED_EDGE('',*,*,#3069,.T.);
#4001=ORIENTED_EDGE('',*,*,#3070,.T.);
#4002=ORIENTED_EDGE('',*,*,#3071,.T.);
#4003=ORIENTED_EDGE('',*,*,#3046,.T.);
#4004=ORIENTED_EDGE('',*,*,#3072,.F.);
#4005=ORIENTED_EDGE('',*,*,#3073,.F.);
#4006=ORIENTED_EDGE('',*,*,#3047,.F.);
#4007=ORIENTED_EDGE('',*,*,#3071,.F.);
#4008=ORIENTED_EDGE('',*,*,#3073,.T.);
#4009=ORIENTED_EDGE('',*,*,#3074,.T.);
#4010=ORIENTED_EDGE('',*,*,#3075,.T.);
#4011=ORIENTED_EDGE('',*,*,#3048,.T.);
#4012=ORIENTED_EDGE('',*,*,#3049,.F.);
#4013=ORIENTED_EDGE('',*,*,#3075,.F.);
#4014=ORIENTED_EDGE('',*,*,#3076,.F.);
#4015=ORIENTED_EDGE('',*,*,#3077,.F.);
#4016=ORIENTED_EDGE('',*,*,#3078,.F.);
#4017=ORIENTED_EDGE('',*,*,#3079,.T.);
#4018=ORIENTED_EDGE('',*,*,#3065,.T.);
#4019=ORIENTED_EDGE('',*,*,#3061,.F.);
#4020=ORIENTED_EDGE('',*,*,#3059,.T.);
#4021=ORIENTED_EDGE('',*,*,#3057,.F.);
#4022=ORIENTED_EDGE('',*,*,#3055,.T.);
#4023=ORIENTED_EDGE('',*,*,#3053,.F.);
#4024=ORIENTED_EDGE('',*,*,#3031,.T.);
#4025=ORIENTED_EDGE('',*,*,#3080,.F.);
#4026=ORIENTED_EDGE('',*,*,#3081,.T.);
#4027=ORIENTED_EDGE('',*,*,#3082,.F.);
#4028=ORIENTED_EDGE('',*,*,#3076,.T.);
#4029=ORIENTED_EDGE('',*,*,#3074,.F.);
#4030=ORIENTED_EDGE('',*,*,#3072,.T.);
#4031=ORIENTED_EDGE('',*,*,#3070,.F.);
#4032=ORIENTED_EDGE('',*,*,#3068,.T.);
#4033=ORIENTED_EDGE('',*,*,#3066,.F.);
#4034=ORIENTED_EDGE('',*,*,#3063,.T.);
#4035=ORIENTED_EDGE('',*,*,#3079,.F.);
#4036=ORIENTED_EDGE('',*,*,#3034,.T.);
#4037=ORIENTED_EDGE('',*,*,#3052,.T.);
#4038=ORIENTED_EDGE('',*,*,#3083,.T.);
#4039=ORIENTED_EDGE('',*,*,#3080,.T.);
#4040=ORIENTED_EDGE('',*,*,#3051,.F.);
#4041=ORIENTED_EDGE('',*,*,#3084,.F.);
#4042=ORIENTED_EDGE('',*,*,#3081,.F.);
#4043=ORIENTED_EDGE('',*,*,#3083,.F.);
#4044=ORIENTED_EDGE('',*,*,#3042,.T.);
#4045=ORIENTED_EDGE('',*,*,#3078,.T.);
#4046=ORIENTED_EDGE('',*,*,#3077,.T.);
#4047=ORIENTED_EDGE('',*,*,#3082,.T.);
#4048=ORIENTED_EDGE('',*,*,#3084,.T.);
#4049=ORIENTED_EDGE('',*,*,#3050,.T.);
#4050=ORIENTED_EDGE('',*,*,#3085,.F.);
#4051=ORIENTED_EDGE('',*,*,#3086,.T.);
#4052=ORIENTED_EDGE('',*,*,#3087,.F.);
#4053=ORIENTED_EDGE('',*,*,#3088,.T.);
#4054=ORIENTED_EDGE('',*,*,#3085,.T.);
#4055=ORIENTED_EDGE('',*,*,#3088,.F.);
#4056=ORIENTED_EDGE('',*,*,#3087,.T.);
#4057=ORIENTED_EDGE('',*,*,#3089,.F.);
#4058=ORIENTED_EDGE('',*,*,#3089,.T.);
#4059=ORIENTED_EDGE('',*,*,#3090,.T.);
#4060=ORIENTED_EDGE('',*,*,#3086,.F.);
#4061=ORIENTED_EDGE('',*,*,#3090,.F.);
#4062=ORIENTED_EDGE('',*,*,#3091,.F.);
#4063=ORIENTED_EDGE('',*,*,#3092,.T.);
#4064=ORIENTED_EDGE('',*,*,#3093,.F.);
#4065=ORIENTED_EDGE('',*,*,#3094,.T.);
#4066=ORIENTED_EDGE('',*,*,#3091,.T.);
#4067=ORIENTED_EDGE('',*,*,#3094,.F.);
#4068=ORIENTED_EDGE('',*,*,#3093,.T.);
#4069=ORIENTED_EDGE('',*,*,#3095,.F.);
#4070=ORIENTED_EDGE('',*,*,#3095,.T.);
#4071=ORIENTED_EDGE('',*,*,#3096,.T.);
#4072=ORIENTED_EDGE('',*,*,#3092,.F.);
#4073=ORIENTED_EDGE('',*,*,#3096,.F.);
#4074=ORIENTED_EDGE('',*,*,#3097,.T.);
#4075=ORIENTED_EDGE('',*,*,#3098,.T.);
#4076=ORIENTED_EDGE('',*,*,#3099,.T.);
#4077=ORIENTED_EDGE('',*,*,#3100,.F.);
#4078=ORIENTED_EDGE('',*,*,#3101,.T.);
#4079=ORIENTED_EDGE('',*,*,#3102,.T.);
#4080=ORIENTED_EDGE('',*,*,#3103,.T.);
#4081=ORIENTED_EDGE('',*,*,#3098,.F.);
#4082=ORIENTED_EDGE('',*,*,#3104,.T.);
#4083=ORIENTED_EDGE('',*,*,#3105,.T.);
#4084=ORIENTED_EDGE('',*,*,#3106,.T.);
#4085=ORIENTED_EDGE('',*,*,#3102,.F.);
#4086=ORIENTED_EDGE('',*,*,#3107,.T.);
#4087=ORIENTED_EDGE('',*,*,#3108,.T.);
#4088=ORIENTED_EDGE('',*,*,#3109,.T.);
#4089=ORIENTED_EDGE('',*,*,#3105,.F.);
#4090=ORIENTED_EDGE('',*,*,#3110,.T.);
#4091=ORIENTED_EDGE('',*,*,#3111,.T.);
#4092=ORIENTED_EDGE('',*,*,#3112,.T.);
#4093=ORIENTED_EDGE('',*,*,#3108,.F.);
#4094=ORIENTED_EDGE('',*,*,#3113,.T.);
#4095=ORIENTED_EDGE('',*,*,#3100,.T.);
#4096=ORIENTED_EDGE('',*,*,#3114,.T.);
#4097=ORIENTED_EDGE('',*,*,#3111,.F.);
#4098=ORIENTED_EDGE('',*,*,#3113,.F.);
#4099=ORIENTED_EDGE('',*,*,#3110,.F.);
#4100=ORIENTED_EDGE('',*,*,#3107,.F.);
#4101=ORIENTED_EDGE('',*,*,#3104,.F.);
#4102=ORIENTED_EDGE('',*,*,#3101,.F.);
#4103=ORIENTED_EDGE('',*,*,#3097,.F.);
#4104=ORIENTED_EDGE('',*,*,#3114,.F.);
#4105=ORIENTED_EDGE('',*,*,#3099,.F.);
#4106=ORIENTED_EDGE('',*,*,#3103,.F.);
#4107=ORIENTED_EDGE('',*,*,#3106,.F.);
#4108=ORIENTED_EDGE('',*,*,#3109,.F.);
#4109=ORIENTED_EDGE('',*,*,#3112,.F.);
#4110=ORIENTED_EDGE('',*,*,#3115,.F.);
#4111=ORIENTED_EDGE('',*,*,#3116,.F.);
#4112=ORIENTED_EDGE('',*,*,#3117,.F.);
#4113=ORIENTED_EDGE('',*,*,#3118,.T.);
#4114=ORIENTED_EDGE('',*,*,#3116,.T.);
#4115=ORIENTED_EDGE('',*,*,#3118,.F.);
#4116=ORIENTED_EDGE('',*,*,#3119,.F.);
#4117=ORIENTED_EDGE('',*,*,#3120,.T.);
#4118=ORIENTED_EDGE('',*,*,#3117,.T.);
#4119=ORIENTED_EDGE('',*,*,#3120,.F.);
#4120=ORIENTED_EDGE('',*,*,#3121,.F.);
#4121=ORIENTED_EDGE('',*,*,#3122,.T.);
#4122=ORIENTED_EDGE('',*,*,#3119,.T.);
#4123=ORIENTED_EDGE('',*,*,#3122,.F.);
#4124=ORIENTED_EDGE('',*,*,#3121,.T.);
#4125=ORIENTED_EDGE('',*,*,#3123,.F.);
#4126=ORIENTED_EDGE('',*,*,#3124,.F.);
#4127=ORIENTED_EDGE('',*,*,#3125,.T.);
#4128=ORIENTED_EDGE('',*,*,#3123,.T.);
#4129=ORIENTED_EDGE('',*,*,#3125,.F.);
#4130=ORIENTED_EDGE('',*,*,#3115,.T.);
#4131=ORIENTED_EDGE('',*,*,#3126,.T.);
#4132=ORIENTED_EDGE('',*,*,#3124,.T.);
#4133=ORIENTED_EDGE('',*,*,#3126,.F.);
#4134=ORIENTED_EDGE('',*,*,#3127,.T.);
#4135=ORIENTED_EDGE('',*,*,#3128,.T.);
#4136=ORIENTED_EDGE('',*,*,#3129,.T.);
#4137=ORIENTED_EDGE('',*,*,#3130,.F.);
#4138=ORIENTED_EDGE('',*,*,#3131,.T.);
#4139=ORIENTED_EDGE('',*,*,#3132,.T.);
#4140=ORIENTED_EDGE('',*,*,#3133,.T.);
#4141=ORIENTED_EDGE('',*,*,#3128,.F.);
#4142=ORIENTED_EDGE('',*,*,#3134,.T.);
#4143=ORIENTED_EDGE('',*,*,#3135,.T.);
#4144=ORIENTED_EDGE('',*,*,#3136,.T.);
#4145=ORIENTED_EDGE('',*,*,#3132,.F.);
#4146=ORIENTED_EDGE('',*,*,#3137,.T.);
#4147=ORIENTED_EDGE('',*,*,#3138,.T.);
#4148=ORIENTED_EDGE('',*,*,#3139,.T.);
#4149=ORIENTED_EDGE('',*,*,#3135,.F.);
#4150=ORIENTED_EDGE('',*,*,#3140,.T.);
#4151=ORIENTED_EDGE('',*,*,#3141,.T.);
#4152=ORIENTED_EDGE('',*,*,#3142,.T.);
#4153=ORIENTED_EDGE('',*,*,#3138,.F.);
#4154=ORIENTED_EDGE('',*,*,#3143,.T.);
#4155=ORIENTED_EDGE('',*,*,#3130,.T.);
#4156=ORIENTED_EDGE('',*,*,#3144,.T.);
#4157=ORIENTED_EDGE('',*,*,#3141,.F.);
#4158=ORIENTED_EDGE('',*,*,#3143,.F.);
#4159=ORIENTED_EDGE('',*,*,#3140,.F.);
#4160=ORIENTED_EDGE('',*,*,#3137,.F.);
#4161=ORIENTED_EDGE('',*,*,#3134,.F.);
#4162=ORIENTED_EDGE('',*,*,#3131,.F.);
#4163=ORIENTED_EDGE('',*,*,#3127,.F.);
#4164=ORIENTED_EDGE('',*,*,#3144,.F.);
#4165=ORIENTED_EDGE('',*,*,#3129,.F.);
#4166=ORIENTED_EDGE('',*,*,#3133,.F.);
#4167=ORIENTED_EDGE('',*,*,#3136,.F.);
#4168=ORIENTED_EDGE('',*,*,#3139,.F.);
#4169=ORIENTED_EDGE('',*,*,#3142,.F.);
#4170=ORIENTED_EDGE('',*,*,#3145,.F.);
#4171=ORIENTED_EDGE('',*,*,#3146,.F.);
#4172=ORIENTED_EDGE('',*,*,#3147,.F.);
#4173=ORIENTED_EDGE('',*,*,#3148,.T.);
#4174=ORIENTED_EDGE('',*,*,#3146,.T.);
#4175=ORIENTED_EDGE('',*,*,#3148,.F.);
#4176=ORIENTED_EDGE('',*,*,#3149,.F.);
#4177=ORIENTED_EDGE('',*,*,#3150,.T.);
#4178=ORIENTED_EDGE('',*,*,#3147,.T.);
#4179=ORIENTED_EDGE('',*,*,#3150,.F.);
#4180=ORIENTED_EDGE('',*,*,#3151,.F.);
#4181=ORIENTED_EDGE('',*,*,#3152,.T.);
#4182=ORIENTED_EDGE('',*,*,#3149,.T.);
#4183=ORIENTED_EDGE('',*,*,#3152,.F.);
#4184=ORIENTED_EDGE('',*,*,#3151,.T.);
#4185=ORIENTED_EDGE('',*,*,#3153,.F.);
#4186=ORIENTED_EDGE('',*,*,#3154,.F.);
#4187=ORIENTED_EDGE('',*,*,#3155,.T.);
#4188=ORIENTED_EDGE('',*,*,#3153,.T.);
#4189=ORIENTED_EDGE('',*,*,#3155,.F.);
#4190=ORIENTED_EDGE('',*,*,#3145,.T.);
#4191=ORIENTED_EDGE('',*,*,#3156,.T.);
#4192=ORIENTED_EDGE('',*,*,#3154,.T.);
#4193=ORIENTED_EDGE('',*,*,#3156,.F.);
#4194=ORIENTED_EDGE('',*,*,#3157,.F.);
#4195=ORIENTED_EDGE('',*,*,#3158,.F.);
#4196=ORIENTED_EDGE('',*,*,#3159,.T.);
#4197=ORIENTED_EDGE('',*,*,#3160,.T.);
#4198=ORIENTED_EDGE('',*,*,#3159,.F.);
#4199=ORIENTED_EDGE('',*,*,#3161,.F.);
#4200=ORIENTED_EDGE('',*,*,#3162,.F.);
#4201=ORIENTED_EDGE('',*,*,#3163,.T.);
#4202=ORIENTED_EDGE('',*,*,#3157,.T.);
#4203=ORIENTED_EDGE('',*,*,#3164,.T.);
#4204=ORIENTED_EDGE('',*,*,#3162,.T.);
#4205=ORIENTED_EDGE('',*,*,#3165,.F.);
#4206=ORIENTED_EDGE('',*,*,#3161,.T.);
#4207=ORIENTED_EDGE('',*,*,#3158,.T.);
#4208=ORIENTED_EDGE('',*,*,#3165,.T.);
#4209=ORIENTED_EDGE('',*,*,#3163,.F.);
#4210=ORIENTED_EDGE('',*,*,#3164,.F.);
#4211=ORIENTED_EDGE('',*,*,#3160,.F.);
#4212=ORIENTED_EDGE('',*,*,#3166,.F.);
#4213=ORIENTED_EDGE('',*,*,#3167,.T.);
#4214=ORIENTED_EDGE('',*,*,#3168,.F.);
#4215=ORIENTED_EDGE('',*,*,#3169,.T.);
#4216=ORIENTED_EDGE('',*,*,#3166,.T.);
#4217=ORIENTED_EDGE('',*,*,#3169,.F.);
#4218=ORIENTED_EDGE('',*,*,#3170,.F.);
#4219=ORIENTED_EDGE('',*,*,#3171,.F.);
#4220=ORIENTED_EDGE('',*,*,#3167,.F.);
#4221=ORIENTED_EDGE('',*,*,#3172,.T.);
#4222=ORIENTED_EDGE('',*,*,#3170,.T.);
#4223=ORIENTED_EDGE('',*,*,#3172,.F.);
#4224=ORIENTED_EDGE('',*,*,#3171,.T.);
#4225=ORIENTED_EDGE('',*,*,#3173,.T.);
#4226=ORIENTED_EDGE('',*,*,#3174,.T.);
#4227=ORIENTED_EDGE('',*,*,#3173,.F.);
#4228=ORIENTED_EDGE('',*,*,#3168,.T.);
#4229=ORIENTED_EDGE('',*,*,#3174,.F.);
#4230=ORIENTED_EDGE('',*,*,#3175,.F.);
#4231=ORIENTED_EDGE('',*,*,#3176,.T.);
#4232=ORIENTED_EDGE('',*,*,#3177,.T.);
#4233=ORIENTED_EDGE('',*,*,#3176,.F.);
#4234=ORIENTED_EDGE('',*,*,#3178,.F.);
#4235=ORIENTED_EDGE('',*,*,#3179,.T.);
#4236=ORIENTED_EDGE('',*,*,#3180,.T.);
#4237=ORIENTED_EDGE('',*,*,#3179,.F.);
#4238=ORIENTED_EDGE('',*,*,#3178,.T.);
#4239=ORIENTED_EDGE('',*,*,#3175,.T.);
#4240=ORIENTED_EDGE('',*,*,#3180,.F.);
#4241=ORIENTED_EDGE('',*,*,#3177,.F.);
#4242=ORIENTED_EDGE('',*,*,#3181,.F.);
#4243=ORIENTED_EDGE('',*,*,#3182,.T.);
#4244=ORIENTED_EDGE('',*,*,#3183,.F.);
#4245=ORIENTED_EDGE('',*,*,#3184,.F.);
#4246=ORIENTED_EDGE('',*,*,#3185,.F.);
#4247=ORIENTED_EDGE('',*,*,#3186,.T.);
#4248=ORIENTED_EDGE('',*,*,#3187,.F.);
#4249=ORIENTED_EDGE('',*,*,#3188,.F.);
#4250=ORIENTED_EDGE('',*,*,#3186,.F.);
#4251=ORIENTED_EDGE('',*,*,#3189,.F.);
#4252=ORIENTED_EDGE('',*,*,#3182,.F.);
#4253=ORIENTED_EDGE('',*,*,#3190,.F.);
#4254=ORIENTED_EDGE('',*,*,#3184,.T.);
#4255=ORIENTED_EDGE('',*,*,#3191,.F.);
#4256=ORIENTED_EDGE('',*,*,#3192,.T.);
#4257=ORIENTED_EDGE('',*,*,#3193,.T.);
#4258=ORIENTED_EDGE('',*,*,#3192,.F.);
#4259=ORIENTED_EDGE('',*,*,#3189,.T.);
#4260=ORIENTED_EDGE('',*,*,#3185,.T.);
#4261=ORIENTED_EDGE('',*,*,#3190,.T.);
#4262=ORIENTED_EDGE('',*,*,#3183,.T.);
#4263=ORIENTED_EDGE('',*,*,#3181,.T.);
#4264=ORIENTED_EDGE('',*,*,#3194,.F.);
#4265=ORIENTED_EDGE('',*,*,#3195,.T.);
#4266=ORIENTED_EDGE('',*,*,#3196,.T.);
#4267=ORIENTED_EDGE('',*,*,#3195,.F.);
#4268=ORIENTED_EDGE('',*,*,#3187,.T.);
#4269=ORIENTED_EDGE('',*,*,#3188,.T.);
#4270=ORIENTED_EDGE('',*,*,#3194,.T.);
#4271=ORIENTED_EDGE('',*,*,#3191,.T.);
#4272=ORIENTED_EDGE('',*,*,#3196,.F.);
#4273=ORIENTED_EDGE('',*,*,#3193,.F.);
#4274=ORIENTED_EDGE('',*,*,#3197,.F.);
#4275=ORIENTED_EDGE('',*,*,#3198,.F.);
#4276=ORIENTED_EDGE('',*,*,#3199,.T.);
#4277=ORIENTED_EDGE('',*,*,#3200,.T.);
#4278=ORIENTED_EDGE('',*,*,#3201,.F.);
#4279=ORIENTED_EDGE('',*,*,#3202,.F.);
#4280=ORIENTED_EDGE('',*,*,#3203,.T.);
#4281=ORIENTED_EDGE('',*,*,#3204,.T.);
#4282=ORIENTED_EDGE('',*,*,#3199,.F.);
#4283=ORIENTED_EDGE('',*,*,#3205,.F.);
#4284=ORIENTED_EDGE('',*,*,#3206,.T.);
#4285=ORIENTED_EDGE('',*,*,#3207,.T.);
#4286=ORIENTED_EDGE('',*,*,#3203,.F.);
#4287=ORIENTED_EDGE('',*,*,#3208,.F.);
#4288=ORIENTED_EDGE('',*,*,#3209,.T.);
#4289=ORIENTED_EDGE('',*,*,#3210,.T.);
#4290=ORIENTED_EDGE('',*,*,#3206,.F.);
#4291=ORIENTED_EDGE('',*,*,#3211,.F.);
#4292=ORIENTED_EDGE('',*,*,#3212,.T.);
#4293=ORIENTED_EDGE('',*,*,#3213,.T.);
#4294=ORIENTED_EDGE('',*,*,#3209,.F.);
#4295=ORIENTED_EDGE('',*,*,#3214,.F.);
#4296=ORIENTED_EDGE('',*,*,#3201,.T.);
#4297=ORIENTED_EDGE('',*,*,#3215,.T.);
#4298=ORIENTED_EDGE('',*,*,#3212,.F.);
#4299=ORIENTED_EDGE('',*,*,#3215,.F.);
#4300=ORIENTED_EDGE('',*,*,#3200,.F.);
#4301=ORIENTED_EDGE('',*,*,#3204,.F.);
#4302=ORIENTED_EDGE('',*,*,#3207,.F.);
#4303=ORIENTED_EDGE('',*,*,#3210,.F.);
#4304=ORIENTED_EDGE('',*,*,#3213,.F.);
#4305=ORIENTED_EDGE('',*,*,#3216,.F.);
#4306=ORIENTED_EDGE('',*,*,#3198,.T.);
#4307=ORIENTED_EDGE('',*,*,#3214,.T.);
#4308=ORIENTED_EDGE('',*,*,#3211,.T.);
#4309=ORIENTED_EDGE('',*,*,#3208,.T.);
#4310=ORIENTED_EDGE('',*,*,#3205,.T.);
#4311=ORIENTED_EDGE('',*,*,#3202,.T.);
#4312=ORIENTED_EDGE('',*,*,#3217,.F.);
#4313=ORIENTED_EDGE('',*,*,#3218,.T.);
#4314=ORIENTED_EDGE('',*,*,#3216,.T.);
#4315=ORIENTED_EDGE('',*,*,#3218,.F.);
#4316=ORIENTED_EDGE('',*,*,#3197,.T.);
#4317=ORIENTED_EDGE('',*,*,#3219,.T.);
#4318=ORIENTED_EDGE('',*,*,#3217,.T.);
#4319=ORIENTED_EDGE('',*,*,#3219,.F.);
#4320=ORIENTED_EDGE('',*,*,#3220,.F.);
#4321=ORIENTED_EDGE('',*,*,#3221,.T.);
#4322=ORIENTED_EDGE('',*,*,#3222,.F.);
#4323=ORIENTED_EDGE('',*,*,#3223,.F.);
#4324=ORIENTED_EDGE('',*,*,#3224,.T.);
#4325=ORIENTED_EDGE('',*,*,#3225,.F.);
#4326=ORIENTED_EDGE('',*,*,#3226,.F.);
#4327=ORIENTED_EDGE('',*,*,#3224,.F.);
#4328=ORIENTED_EDGE('',*,*,#3227,.F.);
#4329=ORIENTED_EDGE('',*,*,#3228,.F.);
#4330=ORIENTED_EDGE('',*,*,#3221,.F.);
#4331=ORIENTED_EDGE('',*,*,#3229,.F.);
#4332=ORIENTED_EDGE('',*,*,#3227,.T.);
#4333=ORIENTED_EDGE('',*,*,#3223,.T.);
#4334=ORIENTED_EDGE('',*,*,#3230,.F.);
#4335=ORIENTED_EDGE('',*,*,#3231,.T.);
#4336=ORIENTED_EDGE('',*,*,#3232,.F.);
#4337=ORIENTED_EDGE('',*,*,#3231,.F.);
#4338=ORIENTED_EDGE('',*,*,#3225,.T.);
#4339=ORIENTED_EDGE('',*,*,#3226,.T.);
#4340=ORIENTED_EDGE('',*,*,#3230,.T.);
#4341=ORIENTED_EDGE('',*,*,#3233,.T.);
#4342=ORIENTED_EDGE('',*,*,#3234,.F.);
#4343=ORIENTED_EDGE('',*,*,#3235,.T.);
#4344=ORIENTED_EDGE('',*,*,#3233,.F.);
#4345=ORIENTED_EDGE('',*,*,#3235,.F.);
#4346=ORIENTED_EDGE('',*,*,#3228,.T.);
#4347=ORIENTED_EDGE('',*,*,#3229,.T.);
#4348=ORIENTED_EDGE('',*,*,#3222,.T.);
#4349=ORIENTED_EDGE('',*,*,#3220,.T.);
#4350=ORIENTED_EDGE('',*,*,#3236,.F.);
#4351=ORIENTED_EDGE('',*,*,#3237,.T.);
#4352=ORIENTED_EDGE('',*,*,#3238,.F.);
#4353=ORIENTED_EDGE('',*,*,#3239,.F.);
#4354=ORIENTED_EDGE('',*,*,#3240,.F.);
#4355=ORIENTED_EDGE('',*,*,#3239,.T.);
#4356=ORIENTED_EDGE('',*,*,#3241,.F.);
#4357=ORIENTED_EDGE('',*,*,#3242,.F.);
#4358=ORIENTED_EDGE('',*,*,#3243,.F.);
#4359=ORIENTED_EDGE('',*,*,#3242,.T.);
#4360=ORIENTED_EDGE('',*,*,#3244,.F.);
#4361=ORIENTED_EDGE('',*,*,#3245,.F.);
#4362=ORIENTED_EDGE('',*,*,#3246,.F.);
#4363=ORIENTED_EDGE('',*,*,#3245,.T.);
#4364=ORIENTED_EDGE('',*,*,#3247,.F.);
#4365=ORIENTED_EDGE('',*,*,#3248,.F.);
#4366=ORIENTED_EDGE('',*,*,#3249,.F.);
#4367=ORIENTED_EDGE('',*,*,#3248,.T.);
#4368=ORIENTED_EDGE('',*,*,#3250,.F.);
#4369=ORIENTED_EDGE('',*,*,#3251,.F.);
#4370=ORIENTED_EDGE('',*,*,#3252,.F.);
#4371=ORIENTED_EDGE('',*,*,#3251,.T.);
#4372=ORIENTED_EDGE('',*,*,#3253,.F.);
#4373=ORIENTED_EDGE('',*,*,#3254,.F.);
#4374=ORIENTED_EDGE('',*,*,#3255,.F.);
#4375=ORIENTED_EDGE('',*,*,#3254,.T.);
#4376=ORIENTED_EDGE('',*,*,#3256,.F.);
#4377=ORIENTED_EDGE('',*,*,#3257,.F.);
#4378=ORIENTED_EDGE('',*,*,#3258,.F.);
#4379=ORIENTED_EDGE('',*,*,#3257,.T.);
#4380=ORIENTED_EDGE('',*,*,#3259,.F.);
#4381=ORIENTED_EDGE('',*,*,#3260,.F.);
#4382=ORIENTED_EDGE('',*,*,#3261,.F.);
#4383=ORIENTED_EDGE('',*,*,#3260,.T.);
#4384=ORIENTED_EDGE('',*,*,#3262,.F.);
#4385=ORIENTED_EDGE('',*,*,#3263,.F.);
#4386=ORIENTED_EDGE('',*,*,#3264,.F.);
#4387=ORIENTED_EDGE('',*,*,#3263,.T.);
#4388=ORIENTED_EDGE('',*,*,#3265,.F.);
#4389=ORIENTED_EDGE('',*,*,#3266,.F.);
#4390=ORIENTED_EDGE('',*,*,#3267,.F.);
#4391=ORIENTED_EDGE('',*,*,#3266,.T.);
#4392=ORIENTED_EDGE('',*,*,#3268,.F.);
#4393=ORIENTED_EDGE('',*,*,#3269,.F.);
#4394=ORIENTED_EDGE('',*,*,#3270,.F.);
#4395=ORIENTED_EDGE('',*,*,#3269,.T.);
#4396=ORIENTED_EDGE('',*,*,#3271,.F.);
#4397=ORIENTED_EDGE('',*,*,#3272,.F.);
#4398=ORIENTED_EDGE('',*,*,#3273,.F.);
#4399=ORIENTED_EDGE('',*,*,#3272,.T.);
#4400=ORIENTED_EDGE('',*,*,#3274,.F.);
#4401=ORIENTED_EDGE('',*,*,#3275,.F.);
#4402=ORIENTED_EDGE('',*,*,#3276,.F.);
#4403=ORIENTED_EDGE('',*,*,#3275,.T.);
#4404=ORIENTED_EDGE('',*,*,#3277,.F.);
#4405=ORIENTED_EDGE('',*,*,#3278,.F.);
#4406=ORIENTED_EDGE('',*,*,#3279,.F.);
#4407=ORIENTED_EDGE('',*,*,#3278,.T.);
#4408=ORIENTED_EDGE('',*,*,#3280,.F.);
#4409=ORIENTED_EDGE('',*,*,#3281,.F.);
#4410=ORIENTED_EDGE('',*,*,#3282,.F.);
#4411=ORIENTED_EDGE('',*,*,#3281,.T.);
#4412=ORIENTED_EDGE('',*,*,#3283,.F.);
#4413=ORIENTED_EDGE('',*,*,#3284,.F.);
#4414=ORIENTED_EDGE('',*,*,#3285,.F.);
#4415=ORIENTED_EDGE('',*,*,#3284,.T.);
#4416=ORIENTED_EDGE('',*,*,#3286,.F.);
#4417=ORIENTED_EDGE('',*,*,#3287,.F.);
#4418=ORIENTED_EDGE('',*,*,#3288,.F.);
#4419=ORIENTED_EDGE('',*,*,#3287,.T.);
#4420=ORIENTED_EDGE('',*,*,#3289,.F.);
#4421=ORIENTED_EDGE('',*,*,#3290,.F.);
#4422=ORIENTED_EDGE('',*,*,#3291,.F.);
#4423=ORIENTED_EDGE('',*,*,#3290,.T.);
#4424=ORIENTED_EDGE('',*,*,#3292,.F.);
#4425=ORIENTED_EDGE('',*,*,#3293,.F.);
#4426=ORIENTED_EDGE('',*,*,#3294,.F.);
#4427=ORIENTED_EDGE('',*,*,#3293,.T.);
#4428=ORIENTED_EDGE('',*,*,#3295,.F.);
#4429=ORIENTED_EDGE('',*,*,#3296,.F.);
#4430=ORIENTED_EDGE('',*,*,#3297,.F.);
#4431=ORIENTED_EDGE('',*,*,#3296,.T.);
#4432=ORIENTED_EDGE('',*,*,#3298,.F.);
#4433=ORIENTED_EDGE('',*,*,#3299,.F.);
#4434=ORIENTED_EDGE('',*,*,#3300,.F.);
#4435=ORIENTED_EDGE('',*,*,#3299,.T.);
#4436=ORIENTED_EDGE('',*,*,#3301,.F.);
#4437=ORIENTED_EDGE('',*,*,#3302,.F.);
#4438=ORIENTED_EDGE('',*,*,#3303,.F.);
#4439=ORIENTED_EDGE('',*,*,#3302,.T.);
#4440=ORIENTED_EDGE('',*,*,#3304,.F.);
#4441=ORIENTED_EDGE('',*,*,#3305,.F.);
#4442=ORIENTED_EDGE('',*,*,#3306,.F.);
#4443=ORIENTED_EDGE('',*,*,#3305,.T.);
#4444=ORIENTED_EDGE('',*,*,#3307,.F.);
#4445=ORIENTED_EDGE('',*,*,#3308,.F.);
#4446=ORIENTED_EDGE('',*,*,#3309,.F.);
#4447=ORIENTED_EDGE('',*,*,#3308,.T.);
#4448=ORIENTED_EDGE('',*,*,#3310,.F.);
#4449=ORIENTED_EDGE('',*,*,#3311,.F.);
#4450=ORIENTED_EDGE('',*,*,#3312,.F.);
#4451=ORIENTED_EDGE('',*,*,#3311,.T.);
#4452=ORIENTED_EDGE('',*,*,#3313,.F.);
#4453=ORIENTED_EDGE('',*,*,#3314,.F.);
#4454=ORIENTED_EDGE('',*,*,#3315,.F.);
#4455=ORIENTED_EDGE('',*,*,#3314,.T.);
#4456=ORIENTED_EDGE('',*,*,#3316,.F.);
#4457=ORIENTED_EDGE('',*,*,#3317,.F.);
#4458=ORIENTED_EDGE('',*,*,#3318,.F.);
#4459=ORIENTED_EDGE('',*,*,#3317,.T.);
#4460=ORIENTED_EDGE('',*,*,#3319,.F.);
#4461=ORIENTED_EDGE('',*,*,#3320,.F.);
#4462=ORIENTED_EDGE('',*,*,#3321,.F.);
#4463=ORIENTED_EDGE('',*,*,#3320,.T.);
#4464=ORIENTED_EDGE('',*,*,#3322,.F.);
#4465=ORIENTED_EDGE('',*,*,#3323,.F.);
#4466=ORIENTED_EDGE('',*,*,#3324,.F.);
#4467=ORIENTED_EDGE('',*,*,#3323,.T.);
#4468=ORIENTED_EDGE('',*,*,#3325,.F.);
#4469=ORIENTED_EDGE('',*,*,#3326,.F.);
#4470=ORIENTED_EDGE('',*,*,#3327,.F.);
#4471=ORIENTED_EDGE('',*,*,#3326,.T.);
#4472=ORIENTED_EDGE('',*,*,#3328,.F.);
#4473=ORIENTED_EDGE('',*,*,#3329,.F.);
#4474=ORIENTED_EDGE('',*,*,#3330,.F.);
#4475=ORIENTED_EDGE('',*,*,#3329,.T.);
#4476=ORIENTED_EDGE('',*,*,#3331,.F.);
#4477=ORIENTED_EDGE('',*,*,#3332,.F.);
#4478=ORIENTED_EDGE('',*,*,#3333,.F.);
#4479=ORIENTED_EDGE('',*,*,#3332,.T.);
#4480=ORIENTED_EDGE('',*,*,#3334,.F.);
#4481=ORIENTED_EDGE('',*,*,#3335,.F.);
#4482=ORIENTED_EDGE('',*,*,#3336,.F.);
#4483=ORIENTED_EDGE('',*,*,#3335,.T.);
#4484=ORIENTED_EDGE('',*,*,#3337,.F.);
#4485=ORIENTED_EDGE('',*,*,#3338,.F.);
#4486=ORIENTED_EDGE('',*,*,#3339,.F.);
#4487=ORIENTED_EDGE('',*,*,#3338,.T.);
#4488=ORIENTED_EDGE('',*,*,#3340,.F.);
#4489=ORIENTED_EDGE('',*,*,#3341,.F.);
#4490=ORIENTED_EDGE('',*,*,#3342,.F.);
#4491=ORIENTED_EDGE('',*,*,#3341,.T.);
#4492=ORIENTED_EDGE('',*,*,#3343,.F.);
#4493=ORIENTED_EDGE('',*,*,#3344,.F.);
#4494=ORIENTED_EDGE('',*,*,#3345,.F.);
#4495=ORIENTED_EDGE('',*,*,#3344,.T.);
#4496=ORIENTED_EDGE('',*,*,#3346,.F.);
#4497=ORIENTED_EDGE('',*,*,#3347,.F.);
#4498=ORIENTED_EDGE('',*,*,#3348,.F.);
#4499=ORIENTED_EDGE('',*,*,#3347,.T.);
#4500=ORIENTED_EDGE('',*,*,#3349,.F.);
#4501=ORIENTED_EDGE('',*,*,#3350,.F.);
#4502=ORIENTED_EDGE('',*,*,#3351,.F.);
#4503=ORIENTED_EDGE('',*,*,#3350,.T.);
#4504=ORIENTED_EDGE('',*,*,#3352,.F.);
#4505=ORIENTED_EDGE('',*,*,#3353,.F.);
#4506=ORIENTED_EDGE('',*,*,#3354,.F.);
#4507=ORIENTED_EDGE('',*,*,#3353,.T.);
#4508=ORIENTED_EDGE('',*,*,#3355,.F.);
#4509=ORIENTED_EDGE('',*,*,#3356,.F.);
#4510=ORIENTED_EDGE('',*,*,#3357,.F.);
#4511=ORIENTED_EDGE('',*,*,#3356,.T.);
#4512=ORIENTED_EDGE('',*,*,#3358,.F.);
#4513=ORIENTED_EDGE('',*,*,#3359,.F.);
#4514=ORIENTED_EDGE('',*,*,#3360,.F.);
#4515=ORIENTED_EDGE('',*,*,#3359,.T.);
#4516=ORIENTED_EDGE('',*,*,#3361,.F.);
#4517=ORIENTED_EDGE('',*,*,#3362,.F.);
#4518=ORIENTED_EDGE('',*,*,#3363,.F.);
#4519=ORIENTED_EDGE('',*,*,#3362,.T.);
#4520=ORIENTED_EDGE('',*,*,#3364,.F.);
#4521=ORIENTED_EDGE('',*,*,#3365,.F.);
#4522=ORIENTED_EDGE('',*,*,#3366,.F.);
#4523=ORIENTED_EDGE('',*,*,#3365,.T.);
#4524=ORIENTED_EDGE('',*,*,#3367,.F.);
#4525=ORIENTED_EDGE('',*,*,#3368,.F.);
#4526=ORIENTED_EDGE('',*,*,#3369,.F.);
#4527=ORIENTED_EDGE('',*,*,#3368,.T.);
#4528=ORIENTED_EDGE('',*,*,#3370,.F.);
#4529=ORIENTED_EDGE('',*,*,#3371,.F.);
#4530=ORIENTED_EDGE('',*,*,#3372,.F.);
#4531=ORIENTED_EDGE('',*,*,#3371,.T.);
#4532=ORIENTED_EDGE('',*,*,#3373,.F.);
#4533=ORIENTED_EDGE('',*,*,#3374,.F.);
#4534=ORIENTED_EDGE('',*,*,#3375,.F.);
#4535=ORIENTED_EDGE('',*,*,#3374,.T.);
#4536=ORIENTED_EDGE('',*,*,#3376,.F.);
#4537=ORIENTED_EDGE('',*,*,#3377,.F.);
#4538=ORIENTED_EDGE('',*,*,#3378,.F.);
#4539=ORIENTED_EDGE('',*,*,#3377,.T.);
#4540=ORIENTED_EDGE('',*,*,#3379,.F.);
#4541=ORIENTED_EDGE('',*,*,#3237,.F.);
#4542=ORIENTED_EDGE('',*,*,#3379,.T.);
#4543=ORIENTED_EDGE('',*,*,#3376,.T.);
#4544=ORIENTED_EDGE('',*,*,#3373,.T.);
#4545=ORIENTED_EDGE('',*,*,#3370,.T.);
#4546=ORIENTED_EDGE('',*,*,#3367,.T.);
#4547=ORIENTED_EDGE('',*,*,#3364,.T.);
#4548=ORIENTED_EDGE('',*,*,#3361,.T.);
#4549=ORIENTED_EDGE('',*,*,#3358,.T.);
#4550=ORIENTED_EDGE('',*,*,#3355,.T.);
#4551=ORIENTED_EDGE('',*,*,#3352,.T.);
#4552=ORIENTED_EDGE('',*,*,#3349,.T.);
#4553=ORIENTED_EDGE('',*,*,#3346,.T.);
#4554=ORIENTED_EDGE('',*,*,#3343,.T.);
#4555=ORIENTED_EDGE('',*,*,#3340,.T.);
#4556=ORIENTED_EDGE('',*,*,#3337,.T.);
#4557=ORIENTED_EDGE('',*,*,#3334,.T.);
#4558=ORIENTED_EDGE('',*,*,#3331,.T.);
#4559=ORIENTED_EDGE('',*,*,#3328,.T.);
#4560=ORIENTED_EDGE('',*,*,#3325,.T.);
#4561=ORIENTED_EDGE('',*,*,#3322,.T.);
#4562=ORIENTED_EDGE('',*,*,#3319,.T.);
#4563=ORIENTED_EDGE('',*,*,#3316,.T.);
#4564=ORIENTED_EDGE('',*,*,#3313,.T.);
#4565=ORIENTED_EDGE('',*,*,#3310,.T.);
#4566=ORIENTED_EDGE('',*,*,#3307,.T.);
#4567=ORIENTED_EDGE('',*,*,#3304,.T.);
#4568=ORIENTED_EDGE('',*,*,#3301,.T.);
#4569=ORIENTED_EDGE('',*,*,#3298,.T.);
#4570=ORIENTED_EDGE('',*,*,#3295,.T.);
#4571=ORIENTED_EDGE('',*,*,#3292,.T.);
#4572=ORIENTED_EDGE('',*,*,#3289,.T.);
#4573=ORIENTED_EDGE('',*,*,#3286,.T.);
#4574=ORIENTED_EDGE('',*,*,#3283,.T.);
#4575=ORIENTED_EDGE('',*,*,#3280,.T.);
#4576=ORIENTED_EDGE('',*,*,#3277,.T.);
#4577=ORIENTED_EDGE('',*,*,#3274,.T.);
#4578=ORIENTED_EDGE('',*,*,#3271,.T.);
#4579=ORIENTED_EDGE('',*,*,#3268,.T.);
#4580=ORIENTED_EDGE('',*,*,#3265,.T.);
#4581=ORIENTED_EDGE('',*,*,#3262,.T.);
#4582=ORIENTED_EDGE('',*,*,#3259,.T.);
#4583=ORIENTED_EDGE('',*,*,#3256,.T.);
#4584=ORIENTED_EDGE('',*,*,#3253,.T.);
#4585=ORIENTED_EDGE('',*,*,#3250,.T.);
#4586=ORIENTED_EDGE('',*,*,#3247,.T.);
#4587=ORIENTED_EDGE('',*,*,#3244,.T.);
#4588=ORIENTED_EDGE('',*,*,#3241,.T.);
#4589=ORIENTED_EDGE('',*,*,#3238,.T.);
#4590=ORIENTED_EDGE('',*,*,#3232,.T.);
#4591=ORIENTED_EDGE('',*,*,#3378,.T.);
#4592=ORIENTED_EDGE('',*,*,#3236,.T.);
#4593=ORIENTED_EDGE('',*,*,#3240,.T.);
#4594=ORIENTED_EDGE('',*,*,#3243,.T.);
#4595=ORIENTED_EDGE('',*,*,#3246,.T.);
#4596=ORIENTED_EDGE('',*,*,#3249,.T.);
#4597=ORIENTED_EDGE('',*,*,#3252,.T.);
#4598=ORIENTED_EDGE('',*,*,#3255,.T.);
#4599=ORIENTED_EDGE('',*,*,#3258,.T.);
#4600=ORIENTED_EDGE('',*,*,#3261,.T.);
#4601=ORIENTED_EDGE('',*,*,#3264,.T.);
#4602=ORIENTED_EDGE('',*,*,#3267,.T.);
#4603=ORIENTED_EDGE('',*,*,#3270,.T.);
#4604=ORIENTED_EDGE('',*,*,#3273,.T.);
#4605=ORIENTED_EDGE('',*,*,#3276,.T.);
#4606=ORIENTED_EDGE('',*,*,#3279,.T.);
#4607=ORIENTED_EDGE('',*,*,#3282,.T.);
#4608=ORIENTED_EDGE('',*,*,#3285,.T.);
#4609=ORIENTED_EDGE('',*,*,#3288,.T.);
#4610=ORIENTED_EDGE('',*,*,#3291,.T.);
#4611=ORIENTED_EDGE('',*,*,#3294,.T.);
#4612=ORIENTED_EDGE('',*,*,#3297,.T.);
#4613=ORIENTED_EDGE('',*,*,#3300,.T.);
#4614=ORIENTED_EDGE('',*,*,#3303,.T.);
#4615=ORIENTED_EDGE('',*,*,#3306,.T.);
#4616=ORIENTED_EDGE('',*,*,#3309,.T.);
#4617=ORIENTED_EDGE('',*,*,#3312,.T.);
#4618=ORIENTED_EDGE('',*,*,#3315,.T.);
#4619=ORIENTED_EDGE('',*,*,#3318,.T.);
#4620=ORIENTED_EDGE('',*,*,#3321,.T.);
#4621=ORIENTED_EDGE('',*,*,#3324,.T.);
#4622=ORIENTED_EDGE('',*,*,#3327,.T.);
#4623=ORIENTED_EDGE('',*,*,#3330,.T.);
#4624=ORIENTED_EDGE('',*,*,#3333,.T.);
#4625=ORIENTED_EDGE('',*,*,#3336,.T.);
#4626=ORIENTED_EDGE('',*,*,#3339,.T.);
#4627=ORIENTED_EDGE('',*,*,#3342,.T.);
#4628=ORIENTED_EDGE('',*,*,#3345,.T.);
#4629=ORIENTED_EDGE('',*,*,#3348,.T.);
#4630=ORIENTED_EDGE('',*,*,#3351,.T.);
#4631=ORIENTED_EDGE('',*,*,#3354,.T.);
#4632=ORIENTED_EDGE('',*,*,#3357,.T.);
#4633=ORIENTED_EDGE('',*,*,#3360,.T.);
#4634=ORIENTED_EDGE('',*,*,#3363,.T.);
#4635=ORIENTED_EDGE('',*,*,#3366,.T.);
#4636=ORIENTED_EDGE('',*,*,#3369,.T.);
#4637=ORIENTED_EDGE('',*,*,#3372,.T.);
#4638=ORIENTED_EDGE('',*,*,#3375,.T.);
#4639=ORIENTED_EDGE('',*,*,#3234,.T.);
#4640=ORIENTED_EDGE('',*,*,#3380,.F.);
#4641=ORIENTED_EDGE('',*,*,#3381,.T.);
#4642=ORIENTED_EDGE('',*,*,#3382,.T.);
#4643=ORIENTED_EDGE('',*,*,#3383,.F.);
#4644=ORIENTED_EDGE('',*,*,#3384,.F.);
#4645=ORIENTED_EDGE('',*,*,#3385,.T.);
#4646=ORIENTED_EDGE('',*,*,#3386,.T.);
#4647=ORIENTED_EDGE('',*,*,#3381,.F.);
#4648=ORIENTED_EDGE('',*,*,#3387,.F.);
#4649=ORIENTED_EDGE('',*,*,#3388,.T.);
#4650=ORIENTED_EDGE('',*,*,#3389,.T.);
#4651=ORIENTED_EDGE('',*,*,#3385,.F.);
#4652=ORIENTED_EDGE('',*,*,#3390,.F.);
#4653=ORIENTED_EDGE('',*,*,#3391,.T.);
#4654=ORIENTED_EDGE('',*,*,#3392,.T.);
#4655=ORIENTED_EDGE('',*,*,#3388,.F.);
#4656=ORIENTED_EDGE('',*,*,#3393,.F.);
#4657=ORIENTED_EDGE('',*,*,#3394,.T.);
#4658=ORIENTED_EDGE('',*,*,#3395,.T.);
#4659=ORIENTED_EDGE('',*,*,#3391,.F.);
#4660=ORIENTED_EDGE('',*,*,#3396,.F.);
#4661=ORIENTED_EDGE('',*,*,#3383,.T.);
#4662=ORIENTED_EDGE('',*,*,#3397,.T.);
#4663=ORIENTED_EDGE('',*,*,#3394,.F.);
#4664=ORIENTED_EDGE('',*,*,#3397,.F.);
#4665=ORIENTED_EDGE('',*,*,#3382,.F.);
#4666=ORIENTED_EDGE('',*,*,#3386,.F.);
#4667=ORIENTED_EDGE('',*,*,#3389,.F.);
#4668=ORIENTED_EDGE('',*,*,#3392,.F.);
#4669=ORIENTED_EDGE('',*,*,#3395,.F.);
#4670=ORIENTED_EDGE('',*,*,#3398,.F.);
#4671=ORIENTED_EDGE('',*,*,#3380,.T.);
#4672=ORIENTED_EDGE('',*,*,#3396,.T.);
#4673=ORIENTED_EDGE('',*,*,#3393,.T.);
#4674=ORIENTED_EDGE('',*,*,#3390,.T.);
#4675=ORIENTED_EDGE('',*,*,#3387,.T.);
#4676=ORIENTED_EDGE('',*,*,#3384,.T.);
#4677=ORIENTED_EDGE('',*,*,#3399,.F.);
#4678=ORIENTED_EDGE('',*,*,#3400,.T.);
#4679=ORIENTED_EDGE('',*,*,#3398,.T.);
#4680=ORIENTED_EDGE('',*,*,#3400,.F.);
#4681=ORIENTED_EDGE('',*,*,#3401,.F.);
#4682=ORIENTED_EDGE('',*,*,#3402,.T.);
#4683=ORIENTED_EDGE('',*,*,#3399,.T.);
#4684=ORIENTED_EDGE('',*,*,#3402,.F.);
#4685=ORIENTED_EDGE('',*,*,#3403,.F.);
#4686=ORIENTED_EDGE('',*,*,#3404,.T.);
#4687=ORIENTED_EDGE('',*,*,#3401,.T.);
#4688=ORIENTED_EDGE('',*,*,#3404,.F.);
#4689=ORIENTED_EDGE('',*,*,#3403,.T.);
#4690=ORIENTED_EDGE('',*,*,#3405,.F.);
#4691=ORIENTED_EDGE('',*,*,#3406,.F.);
#4692=ORIENTED_EDGE('',*,*,#3407,.F.);
#4693=ORIENTED_EDGE('',*,*,#3408,.F.);
#4694=ORIENTED_EDGE('',*,*,#3408,.T.);
#4695=ORIENTED_EDGE('',*,*,#3409,.T.);
#4696=ORIENTED_EDGE('',*,*,#3410,.T.);
#4697=ORIENTED_EDGE('',*,*,#3411,.T.);
#4698=ORIENTED_EDGE('',*,*,#3412,.T.);
#4699=ORIENTED_EDGE('',*,*,#3413,.T.);
#4700=ORIENTED_EDGE('',*,*,#3414,.T.);
#4701=ORIENTED_EDGE('',*,*,#3415,.T.);
#4702=ORIENTED_EDGE('',*,*,#3416,.F.);
#4703=ORIENTED_EDGE('',*,*,#3417,.T.);
#4704=ORIENTED_EDGE('',*,*,#3418,.F.);
#4705=ORIENTED_EDGE('',*,*,#3419,.T.);
#4706=ORIENTED_EDGE('',*,*,#3417,.F.);
#4707=ORIENTED_EDGE('',*,*,#3416,.T.);
#4708=ORIENTED_EDGE('',*,*,#3420,.T.);
#4709=ORIENTED_EDGE('',*,*,#3419,.F.);
#4710=ORIENTED_EDGE('',*,*,#3421,.T.);
#4711=ORIENTED_EDGE('',*,*,#3422,.T.);
#4712=ORIENTED_EDGE('',*,*,#3423,.F.);
#4713=ORIENTED_EDGE('',*,*,#3424,.F.);
#4714=ORIENTED_EDGE('',*,*,#3425,.F.);
#4715=ORIENTED_EDGE('',*,*,#3424,.T.);
#4716=ORIENTED_EDGE('',*,*,#3426,.T.);
#4717=ORIENTED_EDGE('',*,*,#3427,.F.);
#4718=ORIENTED_EDGE('',*,*,#3420,.F.);
#4719=ORIENTED_EDGE('',*,*,#3428,.F.);
#4720=ORIENTED_EDGE('',*,*,#3429,.F.);
#4721=ORIENTED_EDGE('',*,*,#3405,.T.);
#4722=ORIENTED_EDGE('',*,*,#3414,.F.);
#4723=ORIENTED_EDGE('',*,*,#3425,.T.);
#4724=ORIENTED_EDGE('',*,*,#3429,.T.);
#4725=ORIENTED_EDGE('',*,*,#3430,.F.);
#4726=ORIENTED_EDGE('',*,*,#3407,.T.);
#4727=ORIENTED_EDGE('',*,*,#3431,.F.);
#4728=ORIENTED_EDGE('',*,*,#3426,.F.);
#4729=ORIENTED_EDGE('',*,*,#3423,.T.);
#4730=ORIENTED_EDGE('',*,*,#3409,.F.);
#4731=ORIENTED_EDGE('',*,*,#3406,.T.);
#4732=ORIENTED_EDGE('',*,*,#3430,.T.);
#4733=ORIENTED_EDGE('',*,*,#3428,.T.);
#4734=ORIENTED_EDGE('',*,*,#3418,.T.);
#4735=ORIENTED_EDGE('',*,*,#3427,.T.);
#4736=ORIENTED_EDGE('',*,*,#3431,.T.);
#4737=ORIENTED_EDGE('',*,*,#3432,.F.);
#4738=ORIENTED_EDGE('',*,*,#3433,.T.);
#4739=ORIENTED_EDGE('',*,*,#3415,.F.);
#4740=ORIENTED_EDGE('',*,*,#3433,.F.);
#4741=ORIENTED_EDGE('',*,*,#3434,.F.);
#4742=ORIENTED_EDGE('',*,*,#3435,.T.);
#4743=ORIENTED_EDGE('',*,*,#3436,.F.);
#4744=ORIENTED_EDGE('',*,*,#3421,.F.);
#4745=ORIENTED_EDGE('',*,*,#3413,.F.);
#4746=ORIENTED_EDGE('',*,*,#3434,.T.);
#4747=ORIENTED_EDGE('',*,*,#3412,.F.);
#4748=ORIENTED_EDGE('',*,*,#3437,.F.);
#4749=ORIENTED_EDGE('',*,*,#3438,.F.);
#4750=ORIENTED_EDGE('',*,*,#3439,.F.);
#4751=ORIENTED_EDGE('',*,*,#3437,.T.);
#4752=ORIENTED_EDGE('',*,*,#3411,.F.);
#4753=ORIENTED_EDGE('',*,*,#3440,.F.);
#4754=ORIENTED_EDGE('',*,*,#3436,.T.);
#4755=ORIENTED_EDGE('',*,*,#3441,.F.);
#4756=ORIENTED_EDGE('',*,*,#3440,.T.);
#4757=ORIENTED_EDGE('',*,*,#3410,.F.);
#4758=ORIENTED_EDGE('',*,*,#3422,.F.);
#4759=ORIENTED_EDGE('',*,*,#3438,.T.);
#4760=ORIENTED_EDGE('',*,*,#3439,.T.);
#4761=ORIENTED_EDGE('',*,*,#3441,.T.);
#4762=ORIENTED_EDGE('',*,*,#3435,.F.);
#4763=ORIENTED_EDGE('',*,*,#3432,.T.);
#4764=CYLINDRICAL_SURFACE('',#5456,0.225);
#4765=CYLINDRICAL_SURFACE('',#5459,0.210000000000001);
#4766=CYLINDRICAL_SURFACE('',#5462,0.21);
#4767=CYLINDRICAL_SURFACE('',#5465,0.21);
#4768=CYLINDRICAL_SURFACE('',#5468,0.21);
#4769=CYLINDRICAL_SURFACE('',#5471,0.21);
#4770=CYLINDRICAL_SURFACE('',#5474,0.21);
#4771=CYLINDRICAL_SURFACE('',#5484,0.275);
#4772=CYLINDRICAL_SURFACE('',#5487,0.275);
#4773=CYLINDRICAL_SURFACE('',#5490,0.525);
#4774=CYLINDRICAL_SURFACE('',#5495,0.305);
#4775=CYLINDRICAL_SURFACE('',#5497,0.9);
#4776=CYLINDRICAL_SURFACE('',#5508,0.165);
#4777=CYLINDRICAL_SURFACE('',#5515,0.5);
#4778=CYLINDRICAL_SURFACE('',#5518,0.3);
#4779=CYLINDRICAL_SURFACE('',#5522,0.31);
#4780=CYLINDRICAL_SURFACE('',#5525,0.5);
#4781=CYLINDRICAL_SURFACE('',#5531,0.31);
#4782=CYLINDRICAL_SURFACE('',#5534,0.5);
#4783=CYLINDRICAL_SURFACE('',#5540,0.225);
#4784=CYLINDRICAL_SURFACE('',#5543,0.7);
#4785=CYLINDRICAL_SURFACE('',#5549,0.164999999999999);
#4786=CYLINDRICAL_SURFACE('',#5553,0.0999999999999996);
#4787=CYLINDRICAL_SURFACE('',#5566,0.300000000000001);
#4788=CYLINDRICAL_SURFACE('',#5570,0.25);
#4789=CYLINDRICAL_SURFACE('',#5571,0.165);
#4790=CYLINDRICAL_SURFACE('',#5575,0.165);
#4791=CYLINDRICAL_SURFACE('',#5579,0.165);
#4792=CYLINDRICAL_SURFACE('',#5583,0.165);
#4793=CYLINDRICAL_SURFACE('',#5590,0.525);
#4794=CYLINDRICAL_SURFACE('',#5592,0.525);
#4795=CYLINDRICAL_SURFACE('',#5597,0.525);
#4796=CYLINDRICAL_SURFACE('',#5602,0.525);
#4797=CYLINDRICAL_SURFACE('',#5607,2.2);
#4798=CYLINDRICAL_SURFACE('',#5620,0.275);
#4799=CYLINDRICAL_SURFACE('',#5622,0.275);
#4800=CYLINDRICAL_SURFACE('',#5624,0.275);
#4801=CYLINDRICAL_SURFACE('',#5626,0.275);
#4802=CYLINDRICAL_SURFACE('',#5628,1.5);
#4803=CYLINDRICAL_SURFACE('',#5633,3.);
#4804=CYLINDRICAL_SURFACE('',#5635,1.02);
#4805=CYLINDRICAL_SURFACE('',#5640,0.375);
#4806=CYLINDRICAL_SURFACE('',#5645,0.375);
#4807=CYLINDRICAL_SURFACE('',#5650,0.375);
#4808=CYLINDRICAL_SURFACE('',#5655,0.375);
#4809=CYLINDRICAL_SURFACE('',#5660,0.225);
#4810=CYLINDRICAL_SURFACE('',#5662,0.225);
#4811=CYLINDRICAL_SURFACE('',#5664,0.225);
#4812=CYLINDRICAL_SURFACE('',#5666,0.225);
#4813=CYLINDRICAL_SURFACE('',#5668,1.49);
#4814=CYLINDRICAL_SURFACE('',#5673,0.71);
#4815=CYLINDRICAL_SURFACE('',#5675,2.2);
#4816=CYLINDRICAL_SURFACE('',#5688,0.976185);
#4817=CYLINDRICAL_SURFACE('',#5690,0.5);
#4818=CYLINDRICAL_SURFACE('',#5696,0.976185);
#4819=CYLINDRICAL_SURFACE('',#5708,1.023815);
#4820=CYLINDRICAL_SURFACE('',#5715,1.5);
#4821=CYLINDRICAL_SURFACE('',#5720,1.023815);
#4822=CYLINDRICAL_SURFACE('',#5742,1.019052);
#4823=CYLINDRICAL_SURFACE('',#5782,0.980948);
#4824=CYLINDRICAL_SURFACE('',#5796,1.013815);
#4825=CYLINDRICAL_SURFACE('',#5800,0.991185);
#4826=CYLINDRICAL_SURFACE('',#5804,1.013815);
#4827=CYLINDRICAL_SURFACE('',#5808,0.991185);
#4828=CYLINDRICAL_SURFACE('',#5829,0.425);
#4829=CYLINDRICAL_SURFACE('',#5837,0.24505);
#4830=CYLINDRICAL_SURFACE('',#5853,0.35);
#4831=CYLINDRICAL_SURFACE('',#5861,0.1954);
#4832=CYLINDRICAL_SURFACE('',#5899,1.);
#4833=CYLINDRICAL_SURFACE('',#5904,0.7);
#4834=CYLINDRICAL_SURFACE('',#5905,0.5);
#4835=CYLINDRICAL_SURFACE('',#5910,0.505);
#4836=CYLINDRICAL_SURFACE('',#5913,0.7);
#4837=CYLINDRICAL_SURFACE('',#5921,0.165);
#4838=CYLINDRICAL_SURFACE('',#5924,0.505);
#4839=CYLINDRICAL_SURFACE('',#5927,0.9);
#4840=CYLINDRICAL_SURFACE('',#5946,0.1954);
#4841=CYLINDRICAL_SURFACE('',#5950,0.21);
#4842=CYLINDRICAL_SURFACE('',#5954,1.6);
#4843=CYLINDRICAL_SURFACE('',#5959,1.005);
#4844=CYLINDRICAL_SURFACE('',#6023,0.24505);
#4845=CYLINDRICAL_SURFACE('',#6036,0.51);
#4846=CYLINDRICAL_SURFACE('',#6042,0.0999999999999996);
#4847=CYLINDRICAL_SURFACE('',#6054,0.305);
#4848=CYLINDRICAL_SURFACE('',#6056,0.7);
#4849=ADVANCED_FACE('',(#623),#4764,.F.);
#4850=ADVANCED_FACE('',(#624),#4765,.F.);
#4851=ADVANCED_FACE('',(#625),#4766,.F.);
#4852=ADVANCED_FACE('',(#626),#4767,.F.);
#4853=ADVANCED_FACE('',(#627),#4768,.F.);
#4854=ADVANCED_FACE('',(#628),#4769,.F.);
#4855=ADVANCED_FACE('',(#629),#4770,.F.);
#4856=ADVANCED_FACE('',(#630),#437,.T.);
#4857=ADVANCED_FACE('',(#631),#438,.T.);
#4858=ADVANCED_FACE('',(#632),#439,.T.);
#4859=ADVANCED_FACE('',(#633),#440,.T.);
#4860=ADVANCED_FACE('',(#634,#345,#346,#347,#348,#349,#350,#351),#441,.T.);
#4861=ADVANCED_FACE('',(#635,#352,#353,#354,#355,#356,#357,#358),#442,.F.);
#4862=ADVANCED_FACE('',(#636),#4771,.F.);
#4863=ADVANCED_FACE('',(#637),#4772,.F.);
#4864=ADVANCED_FACE('',(#638),#4773,.F.);
#4865=ADVANCED_FACE('',(#639,#359),#443,.F.);
#4866=ADVANCED_FACE('',(#640),#4774,.F.);
#4867=ADVANCED_FACE('',(#641),#4775,.T.);
#4868=ADVANCED_FACE('',(#642,#360),#444,.T.);
#4869=ADVANCED_FACE('',(#643),#445,.T.);
#4870=ADVANCED_FACE('',(#644),#446,.T.);
#4871=ADVANCED_FACE('',(#645),#447,.T.);
#4872=ADVANCED_FACE('',(#646),#448,.T.);
#4873=ADVANCED_FACE('',(#647,#361,#362,#363),#449,.T.);
#4874=ADVANCED_FACE('',(#648,#364,#365,#366),#450,.F.);
#4875=ADVANCED_FACE('',(#649),#4776,.F.);
#4876=ADVANCED_FACE('',(#650),#451,.T.);
#4877=ADVANCED_FACE('',(#651,#367),#452,.T.);
#4878=ADVANCED_FACE('',(#652),#4777,.T.);
#4879=ADVANCED_FACE('',(#653),#453,.F.);
#4880=ADVANCED_FACE('',(#654),#4778,.T.);
#4881=ADVANCED_FACE('',(#655,#368),#454,.T.);
#4882=ADVANCED_FACE('',(#656),#4779,.F.);
#4883=ADVANCED_FACE('',(#657),#4780,.T.);
#4884=ADVANCED_FACE('',(#658,#369),#455,.T.);
#4885=ADVANCED_FACE('',(#659,#370),#456,.F.);
#4886=ADVANCED_FACE('',(#660),#4781,.F.);
#4887=ADVANCED_FACE('',(#661),#4782,.T.);
#4888=ADVANCED_FACE('',(#662,#371),#457,.T.);
#4889=ADVANCED_FACE('',(#663,#372),#458,.F.);
#4890=ADVANCED_FACE('',(#664),#4783,.F.);
#4891=ADVANCED_FACE('',(#665),#4784,.T.);
#4892=ADVANCED_FACE('',(#666,#373),#459,.T.);
#4893=ADVANCED_FACE('',(#667,#374),#460,.F.);
#4894=ADVANCED_FACE('',(#668),#4785,.F.);
#4895=ADVANCED_FACE('',(#669),#461,.F.);
#4896=ADVANCED_FACE('',(#670),#4786,.T.);
#4897=ADVANCED_FACE('',(#671),#462,.T.);
#4898=ADVANCED_FACE('',(#672),#463,.T.);
#4899=ADVANCED_FACE('',(#673),#464,.F.);
#4900=ADVANCED_FACE('',(#674),#465,.T.);
#4901=ADVANCED_FACE('',(#675),#466,.T.);
#4902=ADVANCED_FACE('',(#676),#467,.T.);
#4903=ADVANCED_FACE('',(#677),#468,.T.);
#4904=ADVANCED_FACE('',(#678),#4787,.T.);
#4905=ADVANCED_FACE('',(#679,#375),#469,.F.);
#4906=ADVANCED_FACE('',(#680),#4788,.F.);
#4907=ADVANCED_FACE('',(#681),#4789,.F.);
#4908=ADVANCED_FACE('',(#682),#470,.T.);
#4909=ADVANCED_FACE('',(#683),#4790,.F.);
#4910=ADVANCED_FACE('',(#684),#471,.T.);
#4911=ADVANCED_FACE('',(#685),#4791,.F.);
#4912=ADVANCED_FACE('',(#686),#472,.T.);
#4913=ADVANCED_FACE('',(#687),#4792,.F.);
#4914=ADVANCED_FACE('',(#688),#473,.T.);
#4915=ADVANCED_FACE('',(#689),#474,.F.);
#4916=ADVANCED_FACE('',(#690),#4793,.F.);
#4917=ADVANCED_FACE('',(#691),#4794,.F.);
#4918=ADVANCED_FACE('',(#692),#475,.F.);
#4919=ADVANCED_FACE('',(#693),#4795,.F.);
#4920=ADVANCED_FACE('',(#694),#476,.F.);
#4921=ADVANCED_FACE('',(#695),#4796,.F.);
#4922=ADVANCED_FACE('',(#696),#477,.F.);
#4923=ADVANCED_FACE('',(#697),#4797,.T.);
#4924=ADVANCED_FACE('',(#698,#376,#377,#378,#379,#380),#478,.T.);
#4925=ADVANCED_FACE('',(#699),#4798,.F.);
#4926=ADVANCED_FACE('',(#700),#4799,.F.);
#4927=ADVANCED_FACE('',(#701),#4800,.F.);
#4928=ADVANCED_FACE('',(#702),#4801,.F.);
#4929=ADVANCED_FACE('',(#703),#4802,.F.);
#4930=ADVANCED_FACE('',(#704,#381),#479,.T.);
#4931=ADVANCED_FACE('',(#705,#382),#4803,.T.);
#4932=ADVANCED_FACE('',(#706,#383),#4804,.F.);
#4933=ADVANCED_FACE('',(#707,#384,#385,#386,#387,#388),#480,.T.);
#4934=ADVANCED_FACE('',(#708,#389,#390,#391,#392,#393),#481,.F.);
#4935=ADVANCED_FACE('',(#709),#4805,.F.);
#4936=ADVANCED_FACE('',(#710,#394),#482,.T.);
#4937=ADVANCED_FACE('',(#711),#4806,.F.);
#4938=ADVANCED_FACE('',(#712,#395),#483,.T.);
#4939=ADVANCED_FACE('',(#713),#4807,.F.);
#4940=ADVANCED_FACE('',(#714,#396),#484,.T.);
#4941=ADVANCED_FACE('',(#715),#4808,.F.);
#4942=ADVANCED_FACE('',(#716,#397),#485,.T.);
#4943=ADVANCED_FACE('',(#717),#4809,.F.);
#4944=ADVANCED_FACE('',(#718),#4810,.F.);
#4945=ADVANCED_FACE('',(#719),#4811,.F.);
#4946=ADVANCED_FACE('',(#720),#4812,.F.);
#4947=ADVANCED_FACE('',(#721),#4813,.T.);
#4948=ADVANCED_FACE('',(#722,#398),#486,.F.);
#4949=ADVANCED_FACE('',(#723),#4814,.F.);
#4950=ADVANCED_FACE('',(#724),#4815,.T.);
#4951=ADVANCED_FACE('',(#725,#399,#400,#401,#402,#403),#487,.T.);
#4952=ADVANCED_FACE('',(#726,#404,#405,#406,#407,#408),#488,.F.);
#4953=ADVANCED_FACE('',(#727),#199,.F.);
#4954=ADVANCED_FACE('',(#728),#4816,.T.);
#4955=ADVANCED_FACE('',(#729),#4817,.F.);
#4956=ADVANCED_FACE('',(#730),#186,.F.);
#4957=ADVANCED_FACE('',(#731,#409),#489,.T.);
#4958=ADVANCED_FACE('',(#732),#4818,.T.);
#4959=ADVANCED_FACE('',(#733,#410),#490,.T.);
#4960=ADVANCED_FACE('',(#734),#187,.F.);
#4961=ADVANCED_FACE('',(#735),#200,.F.);
#4962=ADVANCED_FACE('',(#736),#4819,.F.);
#4963=ADVANCED_FACE('',(#737,#411),#491,.T.);
#4964=ADVANCED_FACE('',(#738),#188,.T.);
#4965=ADVANCED_FACE('',(#739),#4820,.T.);
#4966=ADVANCED_FACE('',(#740),#189,.T.);
#4967=ADVANCED_FACE('',(#741,#412),#492,.T.);
#4968=ADVANCED_FACE('',(#742),#4821,.F.);
#4969=ADVANCED_FACE('',(#743),#170,.T.);
#4970=ADVANCED_FACE('',(#744),#171,.T.);
#4971=ADVANCED_FACE('',(#745),#172,.T.);
#4972=ADVANCED_FACE('',(#746),#173,.T.);
#4973=ADVANCED_FACE('',(#747),#174,.T.);
#4974=ADVANCED_FACE('',(#748),#175,.T.);
#4975=ADVANCED_FACE('',(#749),#176,.T.);
#4976=ADVANCED_FACE('',(#750),#177,.T.);
#4977=ADVANCED_FACE('',(#751),#178,.F.);
#4978=ADVANCED_FACE('',(#752),#4822,.T.);
#4979=ADVANCED_FACE('',(#753),#493,.T.);
#4980=ADVANCED_FACE('',(#754),#179,.F.);
#4981=ADVANCED_FACE('',(#755),#494,.T.);
#4982=ADVANCED_FACE('',(#756),#180,.F.);
#4983=ADVANCED_FACE('',(#757),#495,.T.);
#4984=ADVANCED_FACE('',(#758),#181,.F.);
#4985=ADVANCED_FACE('',(#759),#496,.T.);
#4986=ADVANCED_FACE('',(#760),#182,.F.);
#4987=ADVANCED_FACE('',(#761),#497,.T.);
#4988=ADVANCED_FACE('',(#762),#183,.F.);
#4989=ADVANCED_FACE('',(#763),#498,.T.);
#4990=ADVANCED_FACE('',(#764),#184,.F.);
#4991=ADVANCED_FACE('',(#765),#4823,.F.);
#4992=ADVANCED_FACE('',(#766),#499,.T.);
#4993=ADVANCED_FACE('',(#767),#185,.F.);
#4994=ADVANCED_FACE('',(#768,#413),#500,.T.);
#4995=ADVANCED_FACE('',(#769),#501,.T.);
#4996=ADVANCED_FACE('',(#770,#414),#502,.T.);
#4997=ADVANCED_FACE('',(#771),#4824,.T.);
#4998=ADVANCED_FACE('',(#772,#415),#503,.T.);
#4999=ADVANCED_FACE('',(#773),#4825,.F.);
#5000=ADVANCED_FACE('',(#774,#416),#504,.T.);
#5001=ADVANCED_FACE('',(#775),#4826,.T.);
#5002=ADVANCED_FACE('',(#776,#417),#505,.T.);
#5003=ADVANCED_FACE('',(#777),#4827,.F.);
#5004=ADVANCED_FACE('',(#778),#506,.F.);
#5005=ADVANCED_FACE('',(#779),#507,.F.);
#5006=ADVANCED_FACE('',(#780),#508,.F.);
#5007=ADVANCED_FACE('',(#781),#509,.F.);
#5008=ADVANCED_FACE('',(#782),#510,.F.);
#5009=ADVANCED_FACE('',(#783),#511,.F.);
#5010=ADVANCED_FACE('',(#784),#512,.F.);
#5011=ADVANCED_FACE('',(#785),#513,.F.);
#5012=ADVANCED_FACE('',(#786),#514,.F.);
#5013=ADVANCED_FACE('',(#787),#515,.T.);
#5014=ADVANCED_FACE('',(#788),#190,.T.);
#5015=ADVANCED_FACE('',(#789),#4828,.T.);
#5016=ADVANCED_FACE('',(#790),#191,.T.);
#5017=ADVANCED_FACE('',(#791,#418),#516,.T.);
#5018=ADVANCED_FACE('',(#792),#192,.T.);
#5019=ADVANCED_FACE('',(#793),#4829,.T.);
#5020=ADVANCED_FACE('',(#794),#517,.F.);
#5021=ADVANCED_FACE('',(#795),#518,.F.);
#5022=ADVANCED_FACE('',(#796),#519,.F.);
#5023=ADVANCED_FACE('',(#797),#520,.F.);
#5024=ADVANCED_FACE('',(#798),#521,.F.);
#5025=ADVANCED_FACE('',(#799),#522,.F.);
#5026=ADVANCED_FACE('',(#800),#523,.F.);
#5027=ADVANCED_FACE('',(#801),#524,.F.);
#5028=ADVANCED_FACE('',(#802),#525,.F.);
#5029=ADVANCED_FACE('',(#803),#526,.T.);
#5030=ADVANCED_FACE('',(#804),#193,.T.);
#5031=ADVANCED_FACE('',(#805),#4830,.T.);
#5032=ADVANCED_FACE('',(#806),#194,.T.);
#5033=ADVANCED_FACE('',(#807,#419),#527,.T.);
#5034=ADVANCED_FACE('',(#808),#195,.T.);
#5035=ADVANCED_FACE('',(#809),#4831,.T.);
#5036=ADVANCED_FACE('',(#810),#11,.T.);
#5037=ADVANCED_FACE('',(#811),#12,.T.);
#5038=ADVANCED_FACE('',(#812),#13,.T.);
#5039=ADVANCED_FACE('',(#813),#528,.T.);
#5040=ADVANCED_FACE('',(#814),#529,.F.);
#5041=ADVANCED_FACE('',(#815,#420),#530,.F.);
#5042=ADVANCED_FACE('',(#816),#4832,.T.);
#5043=ADVANCED_FACE('',(#817,#421),#531,.F.);
#5044=ADVANCED_FACE('',(#818),#4833,.T.);
#5045=ADVANCED_FACE('',(#819),#4834,.T.);
#5046=ADVANCED_FACE('',(#820),#532,.T.);
#5047=ADVANCED_FACE('',(#821),#533,.F.);
#5048=ADVANCED_FACE('',(#822),#4835,.F.);
#5049=ADVANCED_FACE('',(#823),#4836,.T.);
#5050=ADVANCED_FACE('',(#824,#422),#534,.T.);
#5051=ADVANCED_FACE('',(#825,#423),#535,.F.);
#5052=ADVANCED_FACE('',(#826),#536,.T.);
#5053=ADVANCED_FACE('',(#827),#4837,.F.);
#5054=ADVANCED_FACE('',(#828),#537,.T.);
#5055=ADVANCED_FACE('',(#829,#424),#4838,.F.);
#5056=ADVANCED_FACE('',(#830,#425),#4839,.T.);
#5057=ADVANCED_FACE('',(#831,#426),#538,.T.);
#5058=ADVANCED_FACE('',(#832,#427),#539,.F.);
#5059=ADVANCED_FACE('',(#833),#540,.F.);
#5060=ADVANCED_FACE('',(#834),#541,.F.);
#5061=ADVANCED_FACE('',(#835),#542,.F.);
#5062=ADVANCED_FACE('',(#836),#543,.F.);
#5063=ADVANCED_FACE('',(#837),#544,.F.);
#5064=ADVANCED_FACE('',(#838),#545,.F.);
#5065=ADVANCED_FACE('',(#839),#546,.F.);
#5066=ADVANCED_FACE('',(#840),#547,.F.);
#5067=ADVANCED_FACE('',(#841,#428),#548,.T.);
#5068=ADVANCED_FACE('',(#842),#196,.T.);
#5069=ADVANCED_FACE('',(#843),#4840,.T.);
#5070=ADVANCED_FACE('',(#844),#549,.T.);
#5071=ADVANCED_FACE('',(#845),#4841,.F.);
#5072=ADVANCED_FACE('',(#846),#550,.T.);
#5073=ADVANCED_FACE('',(#847,#429),#4842,.T.);
#5074=ADVANCED_FACE('',(#848,#430),#551,.T.);
#5075=ADVANCED_FACE('',(#849,#431),#4843,.F.);
#5076=ADVANCED_FACE('',(#850),#552,.T.);
#5077=ADVANCED_FACE('',(#851),#553,.T.);
#5078=ADVANCED_FACE('',(#852),#554,.T.);
#5079=ADVANCED_FACE('',(#853),#555,.T.);
#5080=ADVANCED_FACE('',(#854),#556,.T.);
#5081=ADVANCED_FACE('',(#855),#557,.T.);
#5082=ADVANCED_FACE('',(#856),#558,.T.);
#5083=ADVANCED_FACE('',(#857),#559,.T.);
#5084=ADVANCED_FACE('',(#858),#560,.T.);
#5085=ADVANCED_FACE('',(#859),#561,.T.);
#5086=ADVANCED_FACE('',(#860),#562,.T.);
#5087=ADVANCED_FACE('',(#861),#563,.T.);
#5088=ADVANCED_FACE('',(#862),#564,.T.);
#5089=ADVANCED_FACE('',(#863),#565,.T.);
#5090=ADVANCED_FACE('',(#864),#566,.T.);
#5091=ADVANCED_FACE('',(#865),#567,.T.);
#5092=ADVANCED_FACE('',(#866),#568,.T.);
#5093=ADVANCED_FACE('',(#867),#569,.T.);
#5094=ADVANCED_FACE('',(#868),#570,.T.);
#5095=ADVANCED_FACE('',(#869),#571,.T.);
#5096=ADVANCED_FACE('',(#870),#572,.T.);
#5097=ADVANCED_FACE('',(#871),#573,.T.);
#5098=ADVANCED_FACE('',(#872),#574,.T.);
#5099=ADVANCED_FACE('',(#873),#575,.T.);
#5100=ADVANCED_FACE('',(#874),#576,.T.);
#5101=ADVANCED_FACE('',(#875),#577,.T.);
#5102=ADVANCED_FACE('',(#876),#578,.T.);
#5103=ADVANCED_FACE('',(#877),#579,.T.);
#5104=ADVANCED_FACE('',(#878),#580,.T.);
#5105=ADVANCED_FACE('',(#879),#581,.T.);
#5106=ADVANCED_FACE('',(#880),#582,.T.);
#5107=ADVANCED_FACE('',(#881),#583,.T.);
#5108=ADVANCED_FACE('',(#882),#584,.T.);
#5109=ADVANCED_FACE('',(#883),#585,.T.);
#5110=ADVANCED_FACE('',(#884),#586,.T.);
#5111=ADVANCED_FACE('',(#885),#587,.T.);
#5112=ADVANCED_FACE('',(#886),#588,.T.);
#5113=ADVANCED_FACE('',(#887),#589,.T.);
#5114=ADVANCED_FACE('',(#888),#590,.T.);
#5115=ADVANCED_FACE('',(#889),#591,.T.);
#5116=ADVANCED_FACE('',(#890),#592,.T.);
#5117=ADVANCED_FACE('',(#891),#593,.T.);
#5118=ADVANCED_FACE('',(#892),#594,.T.);
#5119=ADVANCED_FACE('',(#893),#595,.T.);
#5120=ADVANCED_FACE('',(#894),#596,.T.);
#5121=ADVANCED_FACE('',(#895),#597,.T.);
#5122=ADVANCED_FACE('',(#896),#598,.T.);
#5123=ADVANCED_FACE('',(#897),#599,.T.);
#5124=ADVANCED_FACE('',(#898,#432),#600,.T.);
#5125=ADVANCED_FACE('',(#899,#433),#601,.F.);
#5126=ADVANCED_FACE('',(#900),#602,.F.);
#5127=ADVANCED_FACE('',(#901),#603,.F.);
#5128=ADVANCED_FACE('',(#902),#604,.F.);
#5129=ADVANCED_FACE('',(#903),#605,.F.);
#5130=ADVANCED_FACE('',(#904),#606,.F.);
#5131=ADVANCED_FACE('',(#905),#607,.F.);
#5132=ADVANCED_FACE('',(#906),#608,.F.);
#5133=ADVANCED_FACE('',(#907,#434),#609,.T.);
#5134=ADVANCED_FACE('',(#908),#197,.T.);
#5135=ADVANCED_FACE('',(#909),#4844,.T.);
#5136=ADVANCED_FACE('',(#910),#198,.T.);
#5137=ADVANCED_FACE('',(#911),#610,.T.);
#5138=ADVANCED_FACE('',(#912),#4845,.F.);
#5139=ADVANCED_FACE('',(#913,#435),#611,.T.);
#5140=ADVANCED_FACE('',(#914),#4846,.T.);
#5141=ADVANCED_FACE('',(#915),#612,.T.);
#5142=ADVANCED_FACE('',(#916),#613,.F.);
#5143=ADVANCED_FACE('',(#917),#614,.F.);
#5144=ADVANCED_FACE('',(#918),#615,.T.);
#5145=ADVANCED_FACE('',(#919),#616,.T.);
#5146=ADVANCED_FACE('',(#920),#617,.T.);
#5147=ADVANCED_FACE('',(#921),#618,.T.);
#5148=ADVANCED_FACE('',(#922),#4847,.F.);
#5149=ADVANCED_FACE('',(#923),#4848,.T.);
#5150=ADVANCED_FACE('',(#924),#619,.T.);
#5151=ADVANCED_FACE('',(#925),#620,.T.);
#5152=ADVANCED_FACE('',(#926),#621,.T.);
#5153=ADVANCED_FACE('',(#927,#436),#622,.F.);
#5154=CLOSED_SHELL('',(#4849,#4850,#4851,#4852,#4853,#4854,#4855,#4856,
#4857,#4858,#4859,#4860,#4861));
#5155=CLOSED_SHELL('',(#4862,#4863,#4864,#4865,#4866,#4867,#4868,#4869,
#4870,#4871,#4872,#4873,#4874));
#5156=CLOSED_SHELL('',(#4875,#4876,#4877,#4878,#4879,#4880,#4881));
#5157=CLOSED_SHELL('',(#4882,#4883,#4884,#4885));
#5158=CLOSED_SHELL('',(#4886,#4887,#4888,#4889));
#5159=CLOSED_SHELL('',(#4890,#4891,#4892,#4893));
#5160=CLOSED_SHELL('',(#4894,#4895,#4896,#4897,#4898,#4899,#4900,#4901,
#4902,#4903,#4904,#4905));
#5161=CLOSED_SHELL('',(#4906,#4907,#4908,#4909,#4910,#4911,#4912,#4913,
#4914,#4915,#4916,#4917,#4918,#4919,#4920,#4921,#4922,#4923,#4924,#4925,
#4926,#4927,#4928,#4929,#4930,#4931,#4932,#4933,#4934));
#5162=CLOSED_SHELL('',(#4935,#4936,#4937,#4938,#4939,#4940,#4941,#4942,
#4943,#4944,#4945,#4946,#4947,#4948,#4949,#4950,#4951,#4952));
#5163=CLOSED_SHELL('',(#4953,#4954,#4955,#4956,#4957,#4958,#4959,#4960));
#5164=CLOSED_SHELL('',(#4961,#4962,#4963,#4964,#4965,#4966,#4967,#4968));
#5165=CLOSED_SHELL('',(#4969));
#5166=CLOSED_SHELL('',(#4970));
#5167=CLOSED_SHELL('',(#4971));
#5168=CLOSED_SHELL('',(#4972));
#5169=CLOSED_SHELL('',(#4973));
#5170=CLOSED_SHELL('',(#4974));
#5171=CLOSED_SHELL('',(#4975));
#5172=CLOSED_SHELL('',(#4976));
#5173=CLOSED_SHELL('',(#4977,#4978,#4979,#4980,#4981,#4982,#4983,#4984,
#4985,#4986,#4987,#4988,#4989,#4990,#4991,#4992,#4993,#4994,#4995));
#5174=CLOSED_SHELL('',(#4996,#4997,#4998,#4999));
#5175=CLOSED_SHELL('',(#5000,#5001,#5002,#5003));
#5176=CLOSED_SHELL('',(#5004,#5005,#5006,#5007,#5008,#5009,#5010,#5011));
#5177=CLOSED_SHELL('',(#5012,#5013,#5014,#5015,#5016,#5017,#5018,#5019));
#5178=CLOSED_SHELL('',(#5020,#5021,#5022,#5023,#5024,#5025,#5026,#5027));
#5179=CLOSED_SHELL('',(#5028,#5029,#5030,#5031,#5032,#5033,#5034,#5035));
#5180=CLOSED_SHELL('',(#5036,#5037,#5038,#5039,#5040));
#5181=CLOSED_SHELL('',(#5041,#5042,#5043,#5044,#5045,#5046,#5047));
#5182=CLOSED_SHELL('',(#5048,#5049,#5050,#5051));
#5183=CLOSED_SHELL('',(#5052,#5053,#5054,#5055,#5056,#5057,#5058));
#5184=CLOSED_SHELL('',(#5059,#5060,#5061,#5062,#5063,#5064,#5065,#5066,
#5067,#5068,#5069));
#5185=CLOSED_SHELL('',(#5070,#5071,#5072,#5073,#5074,#5075,#5076,#5077,
#5078,#5079,#5080,#5081,#5082,#5083,#5084,#5085,#5086,#5087,#5088,#5089,
#5090,#5091,#5092,#5093,#5094,#5095,#5096,#5097,#5098,#5099,#5100,#5101,
#5102,#5103,#5104,#5105,#5106,#5107,#5108,#5109,#5110,#5111,#5112,#5113,
#5114,#5115,#5116,#5117,#5118,#5119,#5120,#5121,#5122,#5123,#5124,#5125));
#5186=CLOSED_SHELL('',(#5126,#5127,#5128,#5129,#5130,#5131,#5132,#5133,
#5134,#5135,#5136,#5137));
#5187=CLOSED_SHELL('',(#5138,#5139,#5140,#5141,#5142,#5143,#5144,#5145,
#5146,#5147,#5148,#5149,#5150,#5151,#5152,#5153));
#5188=DERIVED_UNIT_ELEMENT(#5236,1.);
#5189=DERIVED_UNIT_ELEMENT(#11260,-3.);
#5190=DERIVED_UNIT_ELEMENT(#5236,1.);
#5191=DERIVED_UNIT_ELEMENT(#11260,-3.);
#5192=DERIVED_UNIT_ELEMENT(#5236,1.);
#5193=DERIVED_UNIT_ELEMENT(#11260,-3.);
#5194=DERIVED_UNIT_ELEMENT(#5236,1.);
#5195=DERIVED_UNIT_ELEMENT(#11260,-3.);
#5196=DERIVED_UNIT_ELEMENT(#5236,1.);
#5197=DERIVED_UNIT_ELEMENT(#11260,-3.);
#5198=DERIVED_UNIT_ELEMENT(#5236,1.);
#5199=DERIVED_UNIT_ELEMENT(#11260,-3.);
#5200=DERIVED_UNIT_ELEMENT(#5236,1.);
#5201=DERIVED_UNIT_ELEMENT(#11260,-3.);
#5202=DERIVED_UNIT_ELEMENT(#5236,1.);
#5203=DERIVED_UNIT_ELEMENT(#11260,-3.);
#5204=DERIVED_UNIT_ELEMENT(#5236,1.);
#5205=DERIVED_UNIT_ELEMENT(#11260,-3.);
#5206=DERIVED_UNIT_ELEMENT(#5236,1.);
#5207=DERIVED_UNIT_ELEMENT(#11260,-3.);
#5208=DERIVED_UNIT_ELEMENT(#5236,1.);
#5209=DERIVED_UNIT_ELEMENT(#11260,-3.);
#5210=DERIVED_UNIT_ELEMENT(#5236,1.);
#5211=DERIVED_UNIT_ELEMENT(#11260,-3.);
#5212=DERIVED_UNIT_ELEMENT(#5236,1.);
#5213=DERIVED_UNIT_ELEMENT(#11260,-3.);
#5214=DERIVED_UNIT_ELEMENT(#5236,1.);
#5215=DERIVED_UNIT_ELEMENT(#11260,-3.);
#5216=DERIVED_UNIT_ELEMENT(#5236,1.);
#5217=DERIVED_UNIT_ELEMENT(#11260,-3.);
#5218=DERIVED_UNIT_ELEMENT(#5236,1.);
#5219=DERIVED_UNIT_ELEMENT(#11260,-3.);
#5220=DERIVED_UNIT_ELEMENT(#5236,1.);
#5221=DERIVED_UNIT_ELEMENT(#11260,-3.);
#5222=DERIVED_UNIT_ELEMENT(#5236,1.);
#5223=DERIVED_UNIT_ELEMENT(#11260,-3.);
#5224=DERIVED_UNIT_ELEMENT(#5236,1.);
#5225=DERIVED_UNIT_ELEMENT(#11260,-3.);
#5226=DERIVED_UNIT_ELEMENT(#5236,1.);
#5227=DERIVED_UNIT_ELEMENT(#11260,-3.);
#5228=DERIVED_UNIT_ELEMENT(#5236,1.);
#5229=DERIVED_UNIT_ELEMENT(#11260,-3.);
#5230=DERIVED_UNIT_ELEMENT(#5236,1.);
#5231=DERIVED_UNIT_ELEMENT(#11260,-3.);
#5232=DERIVED_UNIT_ELEMENT(#5236,1.);
#5233=DERIVED_UNIT_ELEMENT(#11260,-3.);
#5234=DERIVED_UNIT_ELEMENT(#5236,1.);
#5235=DERIVED_UNIT_ELEMENT(#11260,-3.);
#5236=(
MASS_UNIT()
NAMED_UNIT(*)
SI_UNIT(.KILO.,.GRAM.)
);
#5237=DERIVED_UNIT((#5188,#5189));
#5238=DERIVED_UNIT((#5190,#5191));
#5239=DERIVED_UNIT((#5192,#5193));
#5240=DERIVED_UNIT((#5194,#5195));
#5241=DERIVED_UNIT((#5196,#5197));
#5242=DERIVED_UNIT((#5198,#5199));
#5243=DERIVED_UNIT((#5200,#5201));
#5244=DERIVED_UNIT((#5202,#5203));
#5245=DERIVED_UNIT((#5204,#5205));
#5246=DERIVED_UNIT((#5206,#5207));
#5247=DERIVED_UNIT((#5208,#5209));
#5248=DERIVED_UNIT((#5210,#5211));
#5249=DERIVED_UNIT((#5212,#5213));
#5250=DERIVED_UNIT((#5214,#5215));
#5251=DERIVED_UNIT((#5216,#5217));
#5252=DERIVED_UNIT((#5218,#5219));
#5253=DERIVED_UNIT((#5220,#5221));
#5254=DERIVED_UNIT((#5222,#5223));
#5255=DERIVED_UNIT((#5224,#5225));
#5256=DERIVED_UNIT((#5226,#5227));
#5257=DERIVED_UNIT((#5228,#5229));
#5258=DERIVED_UNIT((#5230,#5231));
#5259=DERIVED_UNIT((#5232,#5233));
#5260=DERIVED_UNIT((#5234,#5235));
#5261=MEASURE_REPRESENTATION_ITEM('density measure',
POSITIVE_RATIO_MEASURE(7850.),#5237);
#5262=MEASURE_REPRESENTATION_ITEM('density measure',
POSITIVE_RATIO_MEASURE(7850.),#5238);
#5263=MEASURE_REPRESENTATION_ITEM('density measure',
POSITIVE_RATIO_MEASURE(7850.),#5239);
#5264=MEASURE_REPRESENTATION_ITEM('density measure',
POSITIVE_RATIO_MEASURE(7850.),#5240);
#5265=MEASURE_REPRESENTATION_ITEM('density measure',
POSITIVE_RATIO_MEASURE(7850.),#5241);
#5266=MEASURE_REPRESENTATION_ITEM('density measure',
POSITIVE_RATIO_MEASURE(7850.),#5242);
#5267=MEASURE_REPRESENTATION_ITEM('density measure',
POSITIVE_RATIO_MEASURE(7850.),#5243);
#5268=MEASURE_REPRESENTATION_ITEM('density measure',
POSITIVE_RATIO_MEASURE(7850.),#5244);
#5269=MEASURE_REPRESENTATION_ITEM('density measure',
POSITIVE_RATIO_MEASURE(7850.),#5245);
#5270=MEASURE_REPRESENTATION_ITEM('density measure',
POSITIVE_RATIO_MEASURE(7850.),#5246);
#5271=MEASURE_REPRESENTATION_ITEM('density measure',
POSITIVE_RATIO_MEASURE(7850.),#5247);
#5272=MEASURE_REPRESENTATION_ITEM('density measure',
POSITIVE_RATIO_MEASURE(7850.),#5248);
#5273=MEASURE_REPRESENTATION_ITEM('density measure',
POSITIVE_RATIO_MEASURE(7850.),#5249);
#5274=MEASURE_REPRESENTATION_ITEM('density measure',
POSITIVE_RATIO_MEASURE(7850.),#5250);
#5275=MEASURE_REPRESENTATION_ITEM('density measure',
POSITIVE_RATIO_MEASURE(7850.),#5251);
#5276=MEASURE_REPRESENTATION_ITEM('density measure',
POSITIVE_RATIO_MEASURE(7850.),#5252);
#5277=MEASURE_REPRESENTATION_ITEM('density measure',
POSITIVE_RATIO_MEASURE(7850.),#5253);
#5278=MEASURE_REPRESENTATION_ITEM('density measure',
POSITIVE_RATIO_MEASURE(7850.),#5254);
#5279=MEASURE_REPRESENTATION_ITEM('density measure',
POSITIVE_RATIO_MEASURE(7850.),#5255);
#5280=MEASURE_REPRESENTATION_ITEM('density measure',
POSITIVE_RATIO_MEASURE(7850.),#5256);
#5281=MEASURE_REPRESENTATION_ITEM('density measure',
POSITIVE_RATIO_MEASURE(7850.),#5257);
#5282=MEASURE_REPRESENTATION_ITEM('density measure',
POSITIVE_RATIO_MEASURE(7850.),#5258);
#5283=MEASURE_REPRESENTATION_ITEM('density measure',
POSITIVE_RATIO_MEASURE(7850.),#5259);
#5284=MEASURE_REPRESENTATION_ITEM('density measure',
POSITIVE_RATIO_MEASURE(7850.),#5260);
#5285=PROPERTY_DEFINITION_REPRESENTATION(#5405,#5333);
#5286=PROPERTY_DEFINITION_REPRESENTATION(#5406,#5334);
#5287=PROPERTY_DEFINITION_REPRESENTATION(#5407,#5335);
#5288=PROPERTY_DEFINITION_REPRESENTATION(#5408,#5336);
#5289=PROPERTY_DEFINITION_REPRESENTATION(#5409,#5337);
#5290=PROPERTY_DEFINITION_REPRESENTATION(#5410,#5338);
#5291=PROPERTY_DEFINITION_REPRESENTATION(#5411,#5339);
#5292=PROPERTY_DEFINITION_REPRESENTATION(#5412,#5340);
#5293=PROPERTY_DEFINITION_REPRESENTATION(#5413,#5341);
#5294=PROPERTY_DEFINITION_REPRESENTATION(#5414,#5342);
#5295=PROPERTY_DEFINITION_REPRESENTATION(#5415,#5343);
#5296=PROPERTY_DEFINITION_REPRESENTATION(#5416,#5344);
#5297=PROPERTY_DEFINITION_REPRESENTATION(#5417,#5345);
#5298=PROPERTY_DEFINITION_REPRESENTATION(#5418,#5346);
#5299=PROPERTY_DEFINITION_REPRESENTATION(#5419,#5347);
#5300=PROPERTY_DEFINITION_REPRESENTATION(#5420,#5348);
#5301=PROPERTY_DEFINITION_REPRESENTATION(#5421,#5349);
#5302=PROPERTY_DEFINITION_REPRESENTATION(#5422,#5350);
#5303=PROPERTY_DEFINITION_REPRESENTATION(#5423,#5351);
#5304=PROPERTY_DEFINITION_REPRESENTATION(#5424,#5352);
#5305=PROPERTY_DEFINITION_REPRESENTATION(#5425,#5353);
#5306=PROPERTY_DEFINITION_REPRESENTATION(#5426,#5354);
#5307=PROPERTY_DEFINITION_REPRESENTATION(#5427,#5355);
#5308=PROPERTY_DEFINITION_REPRESENTATION(#5428,#5356);
#5309=PROPERTY_DEFINITION_REPRESENTATION(#5429,#5357);
#5310=PROPERTY_DEFINITION_REPRESENTATION(#5430,#5358);
#5311=PROPERTY_DEFINITION_REPRESENTATION(#5431,#5359);
#5312=PROPERTY_DEFINITION_REPRESENTATION(#5432,#5360);
#5313=PROPERTY_DEFINITION_REPRESENTATION(#5433,#5361);
#5314=PROPERTY_DEFINITION_REPRESENTATION(#5434,#5362);
#5315=PROPERTY_DEFINITION_REPRESENTATION(#5435,#5363);
#5316=PROPERTY_DEFINITION_REPRESENTATION(#5436,#5364);
#5317=PROPERTY_DEFINITION_REPRESENTATION(#5437,#5365);
#5318=PROPERTY_DEFINITION_REPRESENTATION(#5438,#5366);
#5319=PROPERTY_DEFINITION_REPRESENTATION(#5439,#5367);
#5320=PROPERTY_DEFINITION_REPRESENTATION(#5440,#5368);
#5321=PROPERTY_DEFINITION_REPRESENTATION(#5441,#5369);
#5322=PROPERTY_DEFINITION_REPRESENTATION(#5442,#5370);
#5323=PROPERTY_DEFINITION_REPRESENTATION(#5443,#5371);
#5324=PROPERTY_DEFINITION_REPRESENTATION(#5444,#5372);
#5325=PROPERTY_DEFINITION_REPRESENTATION(#5445,#5373);
#5326=PROPERTY_DEFINITION_REPRESENTATION(#5446,#5374);
#5327=PROPERTY_DEFINITION_REPRESENTATION(#5447,#5375);
#5328=PROPERTY_DEFINITION_REPRESENTATION(#5448,#5376);
#5329=PROPERTY_DEFINITION_REPRESENTATION(#5449,#5377);
#5330=PROPERTY_DEFINITION_REPRESENTATION(#5450,#5378);
#5331=PROPERTY_DEFINITION_REPRESENTATION(#5451,#5379);
#5332=PROPERTY_DEFINITION_REPRESENTATION(#5452,#5380);
#5333=REPRESENTATION('material name',(#5381),#11231);
#5334=REPRESENTATION('density',(#5261),#11231);
#5335=REPRESENTATION('material name',(#5382),#11232);
#5336=REPRESENTATION('density',(#5262),#11232);
#5337=REPRESENTATION('material name',(#5383),#11233);
#5338=REPRESENTATION('density',(#5263),#11233);
#5339=REPRESENTATION('material name',(#5384),#11234);
#5340=REPRESENTATION('density',(#5264),#11234);
#5341=REPRESENTATION('material name',(#5385),#11235);
#5342=REPRESENTATION('density',(#5265),#11235);
#5343=REPRESENTATION('material name',(#5386),#11236);
#5344=REPRESENTATION('density',(#5266),#11236);
#5345=REPRESENTATION('material name',(#5387),#11237);
#5346=REPRESENTATION('density',(#5267),#11237);
#5347=REPRESENTATION('material name',(#5388),#11238);
#5348=REPRESENTATION('density',(#5268),#11238);
#5349=REPRESENTATION('material name',(#5389),#11239);
#5350=REPRESENTATION('density',(#5269),#11239);
#5351=REPRESENTATION('material name',(#5390),#11241);
#5352=REPRESENTATION('density',(#5270),#11241);
#5353=REPRESENTATION('material name',(#5391),#11242);
#5354=REPRESENTATION('density',(#5271),#11242);
#5355=REPRESENTATION('material name',(#5392),#11243);
#5356=REPRESENTATION('density',(#5272),#11243);
#5357=REPRESENTATION('material name',(#5393),#11244);
#5358=REPRESENTATION('density',(#5273),#11244);
#5359=REPRESENTATION('material name',(#5394),#11245);
#5360=REPRESENTATION('density',(#5274),#11245);
#5361=REPRESENTATION('material name',(#5395),#11246);
#5362=REPRESENTATION('density',(#5275),#11246);
#5363=REPRESENTATION('material name',(#5396),#11247);
#5364=REPRESENTATION('density',(#5276),#11247);
#5365=REPRESENTATION('material name',(#5397),#11248);
#5366=REPRESENTATION('density',(#5277),#11248);
#5367=REPRESENTATION('material name',(#5398),#11250);
#5368=REPRESENTATION('density',(#5278),#11250);
#5369=REPRESENTATION('material name',(#5399),#11251);
#5370=REPRESENTATION('density',(#5279),#11251);
#5371=REPRESENTATION('material name',(#5400),#11252);
#5372=REPRESENTATION('density',(#5280),#11252);
#5373=REPRESENTATION('material name',(#5401),#11253);
#5374=REPRESENTATION('density',(#5281),#11253);
#5375=REPRESENTATION('material name',(#5402),#11254);
#5376=REPRESENTATION('density',(#5282),#11254);
#5377=REPRESENTATION('material name',(#5403),#11255);
#5378=REPRESENTATION('density',(#5283),#11255);
#5379=REPRESENTATION('material name',(#5404),#11257);
#5380=REPRESENTATION('density',(#5284),#11257);
#5381=DESCRIPTIVE_REPRESENTATION_ITEM('Steel','Steel');
#5382=DESCRIPTIVE_REPRESENTATION_ITEM('Steel','Steel');
#5383=DESCRIPTIVE_REPRESENTATION_ITEM('Steel','Steel');
#5384=DESCRIPTIVE_REPRESENTATION_ITEM('Steel','Steel');
#5385=DESCRIPTIVE_REPRESENTATION_ITEM('Steel','Steel');
#5386=DESCRIPTIVE_REPRESENTATION_ITEM('Steel','Steel');
#5387=DESCRIPTIVE_REPRESENTATION_ITEM('Steel','Steel');
#5388=DESCRIPTIVE_REPRESENTATION_ITEM('Steel','Steel');
#5389=DESCRIPTIVE_REPRESENTATION_ITEM('Steel','Steel');
#5390=DESCRIPTIVE_REPRESENTATION_ITEM('Steel','Steel');
#5391=DESCRIPTIVE_REPRESENTATION_ITEM('Steel','Steel');
#5392=DESCRIPTIVE_REPRESENTATION_ITEM('Steel','Steel');
#5393=DESCRIPTIVE_REPRESENTATION_ITEM('Steel','Steel');
#5394=DESCRIPTIVE_REPRESENTATION_ITEM('Steel','Steel');
#5395=DESCRIPTIVE_REPRESENTATION_ITEM('Steel','Steel');
#5396=DESCRIPTIVE_REPRESENTATION_ITEM('Steel','Steel');
#5397=DESCRIPTIVE_REPRESENTATION_ITEM('Steel','Steel');
#5398=DESCRIPTIVE_REPRESENTATION_ITEM('Steel','Steel');
#5399=DESCRIPTIVE_REPRESENTATION_ITEM('Steel','Steel');
#5400=DESCRIPTIVE_REPRESENTATION_ITEM('Steel','Steel');
#5401=DESCRIPTIVE_REPRESENTATION_ITEM('Steel','Steel');
#5402=DESCRIPTIVE_REPRESENTATION_ITEM('Steel','Steel');
#5403=DESCRIPTIVE_REPRESENTATION_ITEM('Steel','Steel');
#5404=DESCRIPTIVE_REPRESENTATION_ITEM('Steel','Steel');
#5405=PROPERTY_DEFINITION('material property','material name',#11391);
#5406=PROPERTY_DEFINITION('material property','density of part',#11391);
#5407=PROPERTY_DEFINITION('material property','material name',#11392);
#5408=PROPERTY_DEFINITION('material property','density of part',#11392);
#5409=PROPERTY_DEFINITION('material property','material name',#11393);
#5410=PROPERTY_DEFINITION('material property','density of part',#11393);
#5411=PROPERTY_DEFINITION('material property','material name',#11394);
#5412=PROPERTY_DEFINITION('material property','density of part',#11394);
#5413=PROPERTY_DEFINITION('material property','material name',#11395);
#5414=PROPERTY_DEFINITION('material property','density of part',#11395);
#5415=PROPERTY_DEFINITION('material property','material name',#11396);
#5416=PROPERTY_DEFINITION('material property','density of part',#11396);
#5417=PROPERTY_DEFINITION('material property','material name',#11397);
#5418=PROPERTY_DEFINITION('material property','density of part',#11397);
#5419=PROPERTY_DEFINITION('material property','material name',#11398);
#5420=PROPERTY_DEFINITION('material property','density of part',#11398);
#5421=PROPERTY_DEFINITION('material property','material name',#11399);
#5422=PROPERTY_DEFINITION('material property','density of part',#11399);
#5423=PROPERTY_DEFINITION('material property','material name',#11401);
#5424=PROPERTY_DEFINITION('material property','density of part',#11401);
#5425=PROPERTY_DEFINITION('material property','material name',#11402);
#5426=PROPERTY_DEFINITION('material property','density of part',#11402);
#5427=PROPERTY_DEFINITION('material property','material name',#11403);
#5428=PROPERTY_DEFINITION('material property','density of part',#11403);
#5429=PROPERTY_DEFINITION('material property','material name',#11404);
#5430=PROPERTY_DEFINITION('material property','density of part',#11404);
#5431=PROPERTY_DEFINITION('material property','material name',#11405);
#5432=PROPERTY_DEFINITION('material property','density of part',#11405);
#5433=PROPERTY_DEFINITION('material property','material name',#11406);
#5434=PROPERTY_DEFINITION('material property','density of part',#11406);
#5435=PROPERTY_DEFINITION('material property','material name',#11407);
#5436=PROPERTY_DEFINITION('material property','density of part',#11407);
#5437=PROPERTY_DEFINITION('material property','material name',#11408);
#5438=PROPERTY_DEFINITION('material property','density of part',#11408);
#5439=PROPERTY_DEFINITION('material property','material name',#11410);
#5440=PROPERTY_DEFINITION('material property','density of part',#11410);
#5441=PROPERTY_DEFINITION('material property','material name',#11411);
#5442=PROPERTY_DEFINITION('material property','density of part',#11411);
#5443=PROPERTY_DEFINITION('material property','material name',#11412);
#5444=PROPERTY_DEFINITION('material property','density of part',#11412);
#5445=PROPERTY_DEFINITION('material property','material name',#11413);
#5446=PROPERTY_DEFINITION('material property','density of part',#11413);
#5447=PROPERTY_DEFINITION('material property','material name',#11414);
#5448=PROPERTY_DEFINITION('material property','density of part',#11414);
#5449=PROPERTY_DEFINITION('material property','material name',#11415);
#5450=PROPERTY_DEFINITION('material property','density of part',#11415);
#5451=PROPERTY_DEFINITION('material property','material name',#11417);
#5452=PROPERTY_DEFINITION('material property','density of part',#11417);
#5453=AXIS2_PLACEMENT_3D('',#7675,#6066,#6067);
#5454=AXIS2_PLACEMENT_3D('',#7676,#6068,#6069);
#5455=AXIS2_PLACEMENT_3D('',#7677,#6070,#6071);
#5456=AXIS2_PLACEMENT_3D('',#7678,#6072,#6073);
#5457=AXIS2_PLACEMENT_3D('',#7680,#6074,#6075);
#5458=AXIS2_PLACEMENT_3D('',#7683,#6077,#6078);
#5459=AXIS2_PLACEMENT_3D('',#7684,#6079,#6080);
#5460=AXIS2_PLACEMENT_3D('',#7686,#6081,#6082);
#5461=AXIS2_PLACEMENT_3D('',#7689,#6084,#6085);
#5462=AXIS2_PLACEMENT_3D('',#7690,#6086,#6087);
#5463=AXIS2_PLACEMENT_3D('',#7692,#6088,#6089);
#5464=AXIS2_PLACEMENT_3D('',#7695,#6091,#6092);
#5465=AXIS2_PLACEMENT_3D('',#7696,#6093,#6094);
#5466=AXIS2_PLACEMENT_3D('',#7698,#6095,#6096);
#5467=AXIS2_PLACEMENT_3D('',#7701,#6098,#6099);
#5468=AXIS2_PLACEMENT_3D('',#7702,#6100,#6101);
#5469=AXIS2_PLACEMENT_3D('',#7704,#6102,#6103);
#5470=AXIS2_PLACEMENT_3D('',#7707,#6105,#6106);
#5471=AXIS2_PLACEMENT_3D('',#7708,#6107,#6108);
#5472=AXIS2_PLACEMENT_3D('',#7710,#6109,#6110);
#5473=AXIS2_PLACEMENT_3D('',#7713,#6112,#6113);
#5474=AXIS2_PLACEMENT_3D('',#7714,#6114,#6115);
#5475=AXIS2_PLACEMENT_3D('',#7716,#6116,#6117);
#5476=AXIS2_PLACEMENT_3D('',#7719,#6119,#6120);
#5477=AXIS2_PLACEMENT_3D('',#7720,#6121,#6122);
#5478=AXIS2_PLACEMENT_3D('',#7729,#6127,#6128);
#5479=AXIS2_PLACEMENT_3D('',#7735,#6132,#6133);
#5480=AXIS2_PLACEMENT_3D('',#7741,#6137,#6138);
#5481=AXIS2_PLACEMENT_3D('',#7744,#6141,#6142);
#5482=AXIS2_PLACEMENT_3D('',#7745,#6143,#6144);
#5483=AXIS2_PLACEMENT_3D('',#7746,#6145,#6146);
#5484=AXIS2_PLACEMENT_3D('',#7747,#6147,#6148);
#5485=AXIS2_PLACEMENT_3D('',#7749,#6149,#6150);
#5486=AXIS2_PLACEMENT_3D('',#7752,#6152,#6153);
#5487=AXIS2_PLACEMENT_3D('',#7753,#6154,#6155);
#5488=AXIS2_PLACEMENT_3D('',#7755,#6156,#6157);
#5489=AXIS2_PLACEMENT_3D('',#7758,#6159,#6160);
#5490=AXIS2_PLACEMENT_3D('',#7759,#6161,#6162);
#5491=AXIS2_PLACEMENT_3D('',#7761,#6163,#6164);
#5492=AXIS2_PLACEMENT_3D('',#7764,#6166,#6167);
#5493=AXIS2_PLACEMENT_3D('',#7765,#6168,#6169);
#5494=AXIS2_PLACEMENT_3D('',#7767,#6170,#6171);
#5495=AXIS2_PLACEMENT_3D('',#7768,#6172,#6173);
#5496=AXIS2_PLACEMENT_3D('',#7771,#6175,#6176);
#5497=AXIS2_PLACEMENT_3D('',#7772,#6177,#6178);
#5498=AXIS2_PLACEMENT_3D('',#7774,#6179,#6180);
#5499=AXIS2_PLACEMENT_3D('',#7777,#6182,#6183);
#5500=AXIS2_PLACEMENT_3D('',#7778,#6184,#6185);
#5501=AXIS2_PLACEMENT_3D('',#7779,#6186,#6187);
#5502=AXIS2_PLACEMENT_3D('',#7788,#6192,#6193);
#5503=AXIS2_PLACEMENT_3D('',#7794,#6197,#6198);
#5504=AXIS2_PLACEMENT_3D('',#7800,#6202,#6203);
#5505=AXIS2_PLACEMENT_3D('',#7803,#6206,#6207);
#5506=AXIS2_PLACEMENT_3D('',#7804,#6208,#6209);
#5507=AXIS2_PLACEMENT_3D('',#7805,#6210,#6211);
#5508=AXIS2_PLACEMENT_3D('',#7806,#6212,#6213);
#5509=AXIS2_PLACEMENT_3D('',#7808,#6214,#6215);
#5510=AXIS2_PLACEMENT_3D('',#7811,#6217,#6218);
#5511=AXIS2_PLACEMENT_3D('',#7812,#6219,#6220);
#5512=AXIS2_PLACEMENT_3D('',#7813,#6221,#6222);
#5513=AXIS2_PLACEMENT_3D('',#7815,#6223,#6224);
#5514=AXIS2_PLACEMENT_3D('',#7817,#6225,#6226);
#5515=AXIS2_PLACEMENT_3D('',#7818,#6227,#6228);
#5516=AXIS2_PLACEMENT_3D('',#7821,#6230,#6231);
#5517=AXIS2_PLACEMENT_3D('',#7822,#6232,#6233);
#5518=AXIS2_PLACEMENT_3D('',#7823,#6234,#6235);
#5519=AXIS2_PLACEMENT_3D('',#7825,#6236,#6237);
#5520=AXIS2_PLACEMENT_3D('',#7827,#6239,#6240);
#5521=AXIS2_PLACEMENT_3D('',#7828,#6241,#6242);
#5522=AXIS2_PLACEMENT_3D('',#7829,#6243,#6244);
#5523=AXIS2_PLACEMENT_3D('',#7831,#6245,#6246);
#5524=AXIS2_PLACEMENT_3D('',#7834,#6248,#6249);
#5525=AXIS2_PLACEMENT_3D('',#7835,#6250,#6251);
#5526=AXIS2_PLACEMENT_3D('',#7837,#6252,#6253);
#5527=AXIS2_PLACEMENT_3D('',#7840,#6255,#6256);
#5528=AXIS2_PLACEMENT_3D('',#7841,#6257,#6258);
#5529=AXIS2_PLACEMENT_3D('',#7842,#6259,#6260);
#5530=AXIS2_PLACEMENT_3D('',#7843,#6261,#6262);
#5531=AXIS2_PLACEMENT_3D('',#7844,#6263,#6264);
#5532=AXIS2_PLACEMENT_3D('',#7846,#6265,#6266);
#5533=AXIS2_PLACEMENT_3D('',#7849,#6268,#6269);
#5534=AXIS2_PLACEMENT_3D('',#7850,#6270,#6271);
#5535=AXIS2_PLACEMENT_3D('',#7852,#6272,#6273);
#5536=AXIS2_PLACEMENT_3D('',#7855,#6275,#6276);
#5537=AXIS2_PLACEMENT_3D('',#7856,#6277,#6278);
#5538=AXIS2_PLACEMENT_3D('',#7857,#6279,#6280);
#5539=AXIS2_PLACEMENT_3D('',#7858,#6281,#6282);
#5540=AXIS2_PLACEMENT_3D('',#7859,#6283,#6284);
#5541=AXIS2_PLACEMENT_3D('',#7861,#6285,#6286);
#5542=AXIS2_PLACEMENT_3D('',#7864,#6288,#6289);
#5543=AXIS2_PLACEMENT_3D('',#7865,#6290,#6291);
#5544=AXIS2_PLACEMENT_3D('',#7867,#6292,#6293);
#5545=AXIS2_PLACEMENT_3D('',#7870,#6295,#6296);
#5546=AXIS2_PLACEMENT_3D('',#7871,#6297,#6298);
#5547=AXIS2_PLACEMENT_3D('',#7872,#6299,#6300);
#5548=AXIS2_PLACEMENT_3D('',#7873,#6301,#6302);
#5549=AXIS2_PLACEMENT_3D('',#7874,#6303,#6304);
#5550=AXIS2_PLACEMENT_3D('',#7876,#6305,#6306);
#5551=AXIS2_PLACEMENT_3D('',#7879,#6308,#6309);
#5552=AXIS2_PLACEMENT_3D('',#7880,#6310,#6311);
#5553=AXIS2_PLACEMENT_3D('',#7881,#6312,#6313);
#5554=AXIS2_PLACEMENT_3D('',#7883,#6314,#6315);
#5555=AXIS2_PLACEMENT_3D('',#7887,#6317,#6318);
#5556=AXIS2_PLACEMENT_3D('',#7888,#6319,#6320);
#5557=AXIS2_PLACEMENT_3D('',#7889,#6321,#6322);
#5558=AXIS2_PLACEMENT_3D('',#7890,#6323,#6324);
#5559=AXIS2_PLACEMENT_3D('',#7900,#6330,#6331);
#5560=AXIS2_PLACEMENT_3D('',#7909,#6335,#6336);
#5561=AXIS2_PLACEMENT_3D('',#7910,#6337,#6338);
#5562=AXIS2_PLACEMENT_3D('',#7914,#6341,#6342);
#5563=AXIS2_PLACEMENT_3D('',#7917,#6345,#6346);
#5564=AXIS2_PLACEMENT_3D('',#7919,#6348,#6349);
#5565=AXIS2_PLACEMENT_3D('',#7921,#6351,#6352);
#5566=AXIS2_PLACEMENT_3D('',#7922,#6353,#6354);
#5567=AXIS2_PLACEMENT_3D('',#7925,#6356,#6357);
#5568=AXIS2_PLACEMENT_3D('',#7926,#6358,#6359);
#5569=AXIS2_PLACEMENT_3D('',#7927,#6360,#6361);
#5570=AXIS2_PLACEMENT_3D('',#7928,#6362,#6363);
#5571=AXIS2_PLACEMENT_3D('',#8006,#6365,#6366);
#5572=AXIS2_PLACEMENT_3D('',#8008,#6367,#6368);
#5573=AXIS2_PLACEMENT_3D('',#8011,#6370,#6371);
#5574=AXIS2_PLACEMENT_3D('',#8012,#6372,#6373);
#5575=AXIS2_PLACEMENT_3D('',#8013,#6374,#6375);
#5576=AXIS2_PLACEMENT_3D('',#8015,#6376,#6377);
#5577=AXIS2_PLACEMENT_3D('',#8018,#6379,#6380);
#5578=AXIS2_PLACEMENT_3D('',#8019,#6381,#6382);
#5579=AXIS2_PLACEMENT_3D('',#8020,#6383,#6384);
#5580=AXIS2_PLACEMENT_3D('',#8022,#6385,#6386);
#5581=AXIS2_PLACEMENT_3D('',#8025,#6388,#6389);
#5582=AXIS2_PLACEMENT_3D('',#8026,#6390,#6391);
#5583=AXIS2_PLACEMENT_3D('',#8027,#6392,#6393);
#5584=AXIS2_PLACEMENT_3D('',#8029,#6394,#6395);
#5585=AXIS2_PLACEMENT_3D('',#8032,#6397,#6398);
#5586=AXIS2_PLACEMENT_3D('',#8033,#6399,#6400);
#5587=AXIS2_PLACEMENT_3D('',#8034,#6401,#6402);
#5588=AXIS2_PLACEMENT_3D('',#8037,#6403,#6404);
#5589=AXIS2_PLACEMENT_3D('',#8038,#6405,#6406);
#5590=AXIS2_PLACEMENT_3D('',#8039,#6407,#6408);
#5591=AXIS2_PLACEMENT_3D('',#8043,#6410,#6411);
#5592=AXIS2_PLACEMENT_3D('',#8045,#6413,#6414);
#5593=AXIS2_PLACEMENT_3D('',#8050,#6416,#6417);
#5594=AXIS2_PLACEMENT_3D('',#8053,#6419,#6420);
#5595=AXIS2_PLACEMENT_3D('',#8054,#6421,#6422);
#5596=AXIS2_PLACEMENT_3D('',#8055,#6423,#6424);
#5597=AXIS2_PLACEMENT_3D('',#8056,#6425,#6426);
#5598=AXIS2_PLACEMENT_3D('',#8061,#6428,#6429);
#5599=AXIS2_PLACEMENT_3D('',#8064,#6431,#6432);
#5600=AXIS2_PLACEMENT_3D('',#8065,#6433,#6434);
#5601=AXIS2_PLACEMENT_3D('',#8066,#6435,#6436);
#5602=AXIS2_PLACEMENT_3D('',#8067,#6437,#6438);
#5603=AXIS2_PLACEMENT_3D('',#8072,#6440,#6441);
#5604=AXIS2_PLACEMENT_3D('',#8075,#6443,#6444);
#5605=AXIS2_PLACEMENT_3D('',#8076,#6445,#6446);
#5606=AXIS2_PLACEMENT_3D('',#8077,#6447,#6448);
#5607=AXIS2_PLACEMENT_3D('',#8078,#6449,#6450);
#5608=AXIS2_PLACEMENT_3D('',#8080,#6451,#6452);
#5609=AXIS2_PLACEMENT_3D('',#8083,#6454,#6455);
#5610=AXIS2_PLACEMENT_3D('',#8084,#6456,#6457);
#5611=AXIS2_PLACEMENT_3D('',#8085,#6458,#6459);
#5612=AXIS2_PLACEMENT_3D('',#8086,#6460,#6461);
#5613=AXIS2_PLACEMENT_3D('',#8087,#6462,#6463);
#5614=AXIS2_PLACEMENT_3D('',#8088,#6464,#6465);
#5615=AXIS2_PLACEMENT_3D('',#8090,#6466,#6467);
#5616=AXIS2_PLACEMENT_3D('',#8092,#6468,#6469);
#5617=AXIS2_PLACEMENT_3D('',#8094,#6470,#6471);
#5618=AXIS2_PLACEMENT_3D('',#8096,#6472,#6473);
#5619=AXIS2_PLACEMENT_3D('',#8098,#6474,#6475);
#5620=AXIS2_PLACEMENT_3D('',#8099,#6476,#6477);
#5621=AXIS2_PLACEMENT_3D('',#8101,#6478,#6479);
#5622=AXIS2_PLACEMENT_3D('',#8103,#6481,#6482);
#5623=AXIS2_PLACEMENT_3D('',#8105,#6483,#6484);
#5624=AXIS2_PLACEMENT_3D('',#8107,#6486,#6487);
#5625=AXIS2_PLACEMENT_3D('',#8109,#6488,#6489);
#5626=AXIS2_PLACEMENT_3D('',#8111,#6491,#6492);
#5627=AXIS2_PLACEMENT_3D('',#8113,#6493,#6494);
#5628=AXIS2_PLACEMENT_3D('',#8115,#6496,#6497);
#5629=AXIS2_PLACEMENT_3D('',#8117,#6498,#6499);
#5630=AXIS2_PLACEMENT_3D('',#8120,#6501,#6502);
#5631=AXIS2_PLACEMENT_3D('',#8121,#6503,#6504);
#5632=AXIS2_PLACEMENT_3D('',#8123,#6505,#6506);
#5633=AXIS2_PLACEMENT_3D('',#8124,#6507,#6508);
#5634=AXIS2_PLACEMENT_3D('',#8127,#6510,#6511);
#5635=AXIS2_PLACEMENT_3D('',#8128,#6512,#6513);
#5636=AXIS2_PLACEMENT_3D('',#8131,#6515,#6516);
#5637=AXIS2_PLACEMENT_3D('',#8132,#6517,#6518);
#5638=AXIS2_PLACEMENT_3D('',#8133,#6519,#6520);
#5639=AXIS2_PLACEMENT_3D('',#8134,#6521,#6522);
#5640=AXIS2_PLACEMENT_3D('',#8135,#6523,#6524);
#5641=AXIS2_PLACEMENT_3D('',#8137,#6525,#6526);
#5642=AXIS2_PLACEMENT_3D('',#8140,#6528,#6529);
#5643=AXIS2_PLACEMENT_3D('',#8141,#6530,#6531);
#5644=AXIS2_PLACEMENT_3D('',#8143,#6532,#6533);
#5645=AXIS2_PLACEMENT_3D('',#8144,#6534,#6535);
#5646=AXIS2_PLACEMENT_3D('',#8146,#6536,#6537);
#5647=AXIS2_PLACEMENT_3D('',#8149,#6539,#6540);
#5648=AXIS2_PLACEMENT_3D('',#8150,#6541,#6542);
#5649=AXIS2_PLACEMENT_3D('',#8152,#6543,#6544);
#5650=AXIS2_PLACEMENT_3D('',#8153,#6545,#6546);
#5651=AXIS2_PLACEMENT_3D('',#8155,#6547,#6548);
#5652=AXIS2_PLACEMENT_3D('',#8158,#6550,#6551);
#5653=AXIS2_PLACEMENT_3D('',#8159,#6552,#6553);
#5654=AXIS2_PLACEMENT_3D('',#8161,#6554,#6555);
#5655=AXIS2_PLACEMENT_3D('',#8162,#6556,#6557);
#5656=AXIS2_PLACEMENT_3D('',#8164,#6558,#6559);
#5657=AXIS2_PLACEMENT_3D('',#8167,#6561,#6562);
#5658=AXIS2_PLACEMENT_3D('',#8168,#6563,#6564);
#5659=AXIS2_PLACEMENT_3D('',#8170,#6565,#6566);
#5660=AXIS2_PLACEMENT_3D('',#8171,#6567,#6568);
#5661=AXIS2_PLACEMENT_3D('',#8173,#6569,#6570);
#5662=AXIS2_PLACEMENT_3D('',#8175,#6572,#6573);
#5663=AXIS2_PLACEMENT_3D('',#8177,#6574,#6575);
#5664=AXIS2_PLACEMENT_3D('',#8179,#6577,#6578);
#5665=AXIS2_PLACEMENT_3D('',#8181,#6579,#6580);
#5666=AXIS2_PLACEMENT_3D('',#8183,#6582,#6583);
#5667=AXIS2_PLACEMENT_3D('',#8185,#6584,#6585);
#5668=AXIS2_PLACEMENT_3D('',#8187,#6587,#6588);
#5669=AXIS2_PLACEMENT_3D('',#8189,#6589,#6590);
#5670=AXIS2_PLACEMENT_3D('',#8192,#6592,#6593);
#5671=AXIS2_PLACEMENT_3D('',#8193,#6594,#6595);
#5672=AXIS2_PLACEMENT_3D('',#8195,#6596,#6597);
#5673=AXIS2_PLACEMENT_3D('',#8196,#6598,#6599);
#5674=AXIS2_PLACEMENT_3D('',#8198,#6600,#6601);
#5675=AXIS2_PLACEMENT_3D('',#8200,#6603,#6604);
#5676=AXIS2_PLACEMENT_3D('',#8202,#6605,#6606);
#5677=AXIS2_PLACEMENT_3D('',#8205,#6608,#6609);
#5678=AXIS2_PLACEMENT_3D('',#8206,#6610,#6611);
#5679=AXIS2_PLACEMENT_3D('',#8207,#6612,#6613);
#5680=AXIS2_PLACEMENT_3D('',#8208,#6614,#6615);
#5681=AXIS2_PLACEMENT_3D('',#8209,#6616,#6617);
#5682=AXIS2_PLACEMENT_3D('',#8210,#6618,#6619);
#5683=AXIS2_PLACEMENT_3D('',#8213,#6620,#6621);
#5684=AXIS2_PLACEMENT_3D('',#8214,#6622,#6623);
#5685=AXIS2_PLACEMENT_3D('',#8216,#6624,#6625);
#5686=AXIS2_PLACEMENT_3D('',#8218,#6626,#6627);
#5687=AXIS2_PLACEMENT_3D('',#8219,#6628,#6629);
#5688=AXIS2_PLACEMENT_3D('',#8220,#6630,#6631);
#5689=AXIS2_PLACEMENT_3D('',#8223,#6633,#6634);
#5690=AXIS2_PLACEMENT_3D('',#8224,#6635,#6636);
#5691=AXIS2_PLACEMENT_3D('',#8226,#6637,#6638);
#5692=AXIS2_PLACEMENT_3D('',#8229,#6640,#6641);
#5693=AXIS2_PLACEMENT_3D('',#8230,#6642,#6643);
#5694=AXIS2_PLACEMENT_3D('',#8233,#6645,#6646);
#5695=AXIS2_PLACEMENT_3D('',#8234,#6647,#6648);
#5696=AXIS2_PLACEMENT_3D('',#8235,#6649,#6650);
#5697=AXIS2_PLACEMENT_3D('',#8237,#6651,#6652);
#5698=AXIS2_PLACEMENT_3D('',#8239,#6654,#6655);
#5699=AXIS2_PLACEMENT_3D('',#8241,#6656,#6657);
#5700=AXIS2_PLACEMENT_3D('',#8242,#6658,#6659);
#5701=AXIS2_PLACEMENT_3D('',#8244,#6661,#6662);
#5702=AXIS2_PLACEMENT_3D('',#8245,#6663,#6664);
#5703=AXIS2_PLACEMENT_3D('',#8248,#6665,#6666);
#5704=AXIS2_PLACEMENT_3D('',#8249,#6667,#6668);
#5705=AXIS2_PLACEMENT_3D('',#8251,#6669,#6670);
#5706=AXIS2_PLACEMENT_3D('',#8253,#6671,#6672);
#5707=AXIS2_PLACEMENT_3D('',#8254,#6673,#6674);
#5708=AXIS2_PLACEMENT_3D('',#8255,#6675,#6676);
#5709=AXIS2_PLACEMENT_3D('',#8257,#6677,#6678);
#5710=AXIS2_PLACEMENT_3D('',#8259,#6680,#6681);
#5711=AXIS2_PLACEMENT_3D('',#8261,#6682,#6683);
#5712=AXIS2_PLACEMENT_3D('',#8263,#6684,#6685);
#5713=AXIS2_PLACEMENT_3D('',#8264,#6686,#6687);
#5714=AXIS2_PLACEMENT_3D('',#8266,#6688,#6689);
#5715=AXIS2_PLACEMENT_3D('',#8268,#6691,#6692);
#5716=AXIS2_PLACEMENT_3D('',#8270,#6693,#6694);
#5717=AXIS2_PLACEMENT_3D('',#8272,#6696,#6697);
#5718=AXIS2_PLACEMENT_3D('',#8274,#6698,#6699);
#5719=AXIS2_PLACEMENT_3D('',#8276,#6701,#6702);
#5720=AXIS2_PLACEMENT_3D('',#8277,#6703,#6704);
#5721=AXIS2_PLACEMENT_3D('',#8279,#6706,#6707);
#5722=AXIS2_PLACEMENT_3D('',#8280,#6708,#6709);
#5723=AXIS2_PLACEMENT_3D('',#8283,#6710,#6711);
#5724=AXIS2_PLACEMENT_3D('',#8284,#6712,#6713);
#5725=AXIS2_PLACEMENT_3D('',#8287,#6714,#6715);
#5726=AXIS2_PLACEMENT_3D('',#8288,#6716,#6717);
#5727=AXIS2_PLACEMENT_3D('',#8291,#6718,#6719);
#5728=AXIS2_PLACEMENT_3D('',#8292,#6720,#6721);
#5729=AXIS2_PLACEMENT_3D('',#8295,#6722,#6723);
#5730=AXIS2_PLACEMENT_3D('',#8296,#6724,#6725);
#5731=AXIS2_PLACEMENT_3D('',#8299,#6726,#6727);
#5732=AXIS2_PLACEMENT_3D('',#8300,#6728,#6729);
#5733=AXIS2_PLACEMENT_3D('',#8303,#6730,#6731);
#5734=AXIS2_PLACEMENT_3D('',#8304,#6732,#6733);
#5735=AXIS2_PLACEMENT_3D('',#8307,#6734,#6735);
#5736=AXIS2_PLACEMENT_3D('',#8308,#6736,#6737);
#5737=AXIS2_PLACEMENT_3D('',#8311,#6738,#6739);
#5738=AXIS2_PLACEMENT_3D('',#8312,#6740,#6741);
#5739=AXIS2_PLACEMENT_3D('',#8313,#6742,#6743);
#5740=AXIS2_PLACEMENT_3D('',#8339,#6744,#6745);
#5741=AXIS2_PLACEMENT_3D('',#8363,#6746,#6747);
#5742=AXIS2_PLACEMENT_3D('',#8364,#6748,#6749);
#5743=AXIS2_PLACEMENT_3D('',#8366,#6750,#6751);
#5744=AXIS2_PLACEMENT_3D('',#8391,#6752,#6753);
#5745=AXIS2_PLACEMENT_3D('',#8416,#6754,#6755);
#5746=AXIS2_PLACEMENT_3D('',#8432,#6757,#6758);
#5747=AXIS2_PLACEMENT_3D('',#8447,#6759,#6760);
#5748=AXIS2_PLACEMENT_3D('',#8472,#6761,#6762);
#5749=AXIS2_PLACEMENT_3D('',#8497,#6763,#6764);
#5750=AXIS2_PLACEMENT_3D('',#8522,#6765,#6766);
#5751=AXIS2_PLACEMENT_3D('',#8546,#6767,#6768);
#5752=AXIS2_PLACEMENT_3D('',#8547,#6769,#6770);
#5753=AXIS2_PLACEMENT_3D('',#8549,#6771,#6772);
#5754=AXIS2_PLACEMENT_3D('',#8550,#6773,#6774);
#5755=AXIS2_PLACEMENT_3D('',#8551,#6775,#6776);
#5756=AXIS2_PLACEMENT_3D('',#8575,#6777,#6778);
#5757=AXIS2_PLACEMENT_3D('',#8576,#6779,#6780);
#5758=AXIS2_PLACEMENT_3D('',#8578,#6781,#6782);
#5759=AXIS2_PLACEMENT_3D('',#8579,#6783,#6784);
#5760=AXIS2_PLACEMENT_3D('',#8580,#6785,#6786);
#5761=AXIS2_PLACEMENT_3D('',#8604,#6787,#6788);
#5762=AXIS2_PLACEMENT_3D('',#8605,#6789,#6790);
#5763=AXIS2_PLACEMENT_3D('',#8607,#6791,#6792);
#5764=AXIS2_PLACEMENT_3D('',#8608,#6793,#6794);
#5765=AXIS2_PLACEMENT_3D('',#8609,#6795,#6796);
#5766=AXIS2_PLACEMENT_3D('',#8624,#6797,#6798);
#5767=AXIS2_PLACEMENT_3D('',#8637,#6799,#6800);
#5768=AXIS2_PLACEMENT_3D('',#8639,#6801,#6802);
#5769=AXIS2_PLACEMENT_3D('',#8640,#6803,#6804);
#5770=AXIS2_PLACEMENT_3D('',#8641,#6805,#6806);
#5771=AXIS2_PLACEMENT_3D('',#8665,#6807,#6808);
#5772=AXIS2_PLACEMENT_3D('',#8666,#6809,#6810);
#5773=AXIS2_PLACEMENT_3D('',#8668,#6811,#6812);
#5774=AXIS2_PLACEMENT_3D('',#8669,#6813,#6814);
#5775=AXIS2_PLACEMENT_3D('',#8670,#6815,#6816);
#5776=AXIS2_PLACEMENT_3D('',#8694,#6817,#6818);
#5777=AXIS2_PLACEMENT_3D('',#8695,#6819,#6820);
#5778=AXIS2_PLACEMENT_3D('',#8697,#6821,#6822);
#5779=AXIS2_PLACEMENT_3D('',#8698,#6823,#6824);
#5780=AXIS2_PLACEMENT_3D('',#8699,#6825,#6826);
#5781=AXIS2_PLACEMENT_3D('',#8723,#6827,#6828);
#5782=AXIS2_PLACEMENT_3D('',#8724,#6829,#6830);
#5783=AXIS2_PLACEMENT_3D('',#8726,#6831,#6832);
#5784=AXIS2_PLACEMENT_3D('',#8729,#6834,#6835);
#5785=AXIS2_PLACEMENT_3D('',#8753,#6836,#6837);
#5786=AXIS2_PLACEMENT_3D('',#8754,#6838,#6839);
#5787=AXIS2_PLACEMENT_3D('',#8755,#6840,#6841);
#5788=AXIS2_PLACEMENT_3D('',#8756,#6842,#6843);
#5789=AXIS2_PLACEMENT_3D('',#8757,#6844,#6845);
#5790=AXIS2_PLACEMENT_3D('',#8758,#6846,#6847);
#5791=AXIS2_PLACEMENT_3D('',#8759,#6848,#6849);
#5792=AXIS2_PLACEMENT_3D('',#8760,#6850,#6851);
#5793=AXIS2_PLACEMENT_3D('',#8761,#6852,#6853);
#5794=AXIS2_PLACEMENT_3D('',#8763,#6854,#6855);
#5795=AXIS2_PLACEMENT_3D('',#8765,#6856,#6857);
#5796=AXIS2_PLACEMENT_3D('',#8766,#6858,#6859);
#5797=AXIS2_PLACEMENT_3D('',#8768,#6860,#6861);
#5798=AXIS2_PLACEMENT_3D('',#8770,#6863,#6864);
#5799=AXIS2_PLACEMENT_3D('',#8772,#6865,#6866);
#5800=AXIS2_PLACEMENT_3D('',#8773,#6867,#6868);
#5801=AXIS2_PLACEMENT_3D('',#8775,#6870,#6871);
#5802=AXIS2_PLACEMENT_3D('',#8777,#6872,#6873);
#5803=AXIS2_PLACEMENT_3D('',#8779,#6874,#6875);
#5804=AXIS2_PLACEMENT_3D('',#8780,#6876,#6877);
#5805=AXIS2_PLACEMENT_3D('',#8782,#6878,#6879);
#5806=AXIS2_PLACEMENT_3D('',#8784,#6881,#6882);
#5807=AXIS2_PLACEMENT_3D('',#8786,#6883,#6884);
#5808=AXIS2_PLACEMENT_3D('',#8787,#6885,#6886);
#5809=AXIS2_PLACEMENT_3D('',#8789,#6888,#6889);
#5810=AXIS2_PLACEMENT_3D('',#8790,#6890,#6891);
#5811=AXIS2_PLACEMENT_3D('',#8791,#6892,#6893);
#5812=AXIS2_PLACEMENT_3D('',#8792,#6894,#6895);
#5813=AXIS2_PLACEMENT_3D('',#8793,#6896,#6897);
#5814=AXIS2_PLACEMENT_3D('',#8794,#6898,#6899);
#5815=AXIS2_PLACEMENT_3D('',#8795,#6900,#6901);
#5816=AXIS2_PLACEMENT_3D('',#8804,#6906,#6907);
#5817=AXIS2_PLACEMENT_3D('',#8810,#6911,#6912);
#5818=AXIS2_PLACEMENT_3D('',#8816,#6916,#6917);
#5819=AXIS2_PLACEMENT_3D('',#8822,#6921,#6922);
#5820=AXIS2_PLACEMENT_3D('',#8828,#6926,#6927);
#5821=AXIS2_PLACEMENT_3D('',#8831,#6930,#6931);
#5822=AXIS2_PLACEMENT_3D('',#8832,#6932,#6933);
#5823=AXIS2_PLACEMENT_3D('',#8833,#6934,#6935);
#5824=AXIS2_PLACEMENT_3D('',#8835,#6936,#6937);
#5825=AXIS2_PLACEMENT_3D('',#8836,#6938,#6939);
#5826=AXIS2_PLACEMENT_3D('',#8838,#6940,#6941);
#5827=AXIS2_PLACEMENT_3D('',#8839,#6942,#6943);
#5828=AXIS2_PLACEMENT_3D('',#8841,#6944,#6945);
#5829=AXIS2_PLACEMENT_3D('',#8843,#6947,#6948);
#5830=AXIS2_PLACEMENT_3D('',#8845,#6949,#6950);
#5831=AXIS2_PLACEMENT_3D('',#8847,#6952,#6953);
#5832=AXIS2_PLACEMENT_3D('',#8849,#6954,#6955);
#5833=AXIS2_PLACEMENT_3D('',#8851,#6957,#6958);
#5834=AXIS2_PLACEMENT_3D('',#8853,#6959,#6960);
#5835=AXIS2_PLACEMENT_3D('',#8854,#6961,#6962);
#5836=AXIS2_PLACEMENT_3D('',#8856,#6963,#6964);
#5837=AXIS2_PLACEMENT_3D('',#8858,#6966,#6967);
#5838=AXIS2_PLACEMENT_3D('',#8860,#6969,#6970);
#5839=AXIS2_PLACEMENT_3D('',#8861,#6971,#6972);
#5840=AXIS2_PLACEMENT_3D('',#8870,#6977,#6978);
#5841=AXIS2_PLACEMENT_3D('',#8876,#6982,#6983);
#5842=AXIS2_PLACEMENT_3D('',#8882,#6987,#6988);
#5843=AXIS2_PLACEMENT_3D('',#8888,#6992,#6993);
#5844=AXIS2_PLACEMENT_3D('',#8894,#6997,#6998);
#5845=AXIS2_PLACEMENT_3D('',#8897,#7001,#7002);
#5846=AXIS2_PLACEMENT_3D('',#8898,#7003,#7004);
#5847=AXIS2_PLACEMENT_3D('',#8899,#7005,#7006);
#5848=AXIS2_PLACEMENT_3D('',#8901,#7007,#7008);
#5849=AXIS2_PLACEMENT_3D('',#8902,#7009,#7010);
#5850=AXIS2_PLACEMENT_3D('',#8904,#7011,#7012);
#5851=AXIS2_PLACEMENT_3D('',#8905,#7013,#7014);
#5852=AXIS2_PLACEMENT_3D('',#8907,#7015,#7016);
#5853=AXIS2_PLACEMENT_3D('',#8909,#7018,#7019);
#5854=AXIS2_PLACEMENT_3D('',#8911,#7020,#7021);
#5855=AXIS2_PLACEMENT_3D('',#8913,#7023,#7024);
#5856=AXIS2_PLACEMENT_3D('',#8915,#7025,#7026);
#5857=AXIS2_PLACEMENT_3D('',#8917,#7028,#7029);
#5858=AXIS2_PLACEMENT_3D('',#8919,#7030,#7031);
#5859=AXIS2_PLACEMENT_3D('',#8920,#7032,#7033);
#5860=AXIS2_PLACEMENT_3D('',#8922,#7034,#7035);
#5861=AXIS2_PLACEMENT_3D('',#8924,#7037,#7038);
#5862=AXIS2_PLACEMENT_3D('',#8926,#7040,#7041);
#5863=AXIS2_PLACEMENT_3D('',#9600,#7042,#7043);
#5864=AXIS2_PLACEMENT_3D('',#9669,#7044,#7045);
#5865=AXIS2_PLACEMENT_3D('',#9955,#7046,#7047);
#5866=AXIS2_PLACEMENT_3D('',#10028,#7048,#7049);
#5867=AXIS2_PLACEMENT_3D('',#10461,#7050,#7051);
#5868=AXIS2_PLACEMENT_3D('',#10462,#7052,#7053);
#5869=AXIS2_PLACEMENT_3D('',#10463,#7054,#7055);
#5870=AXIS2_PLACEMENT_3D('',#10464,#7056,#7057);
#5871=AXIS2_PLACEMENT_3D('',#10465,#7058,#7059);
#5872=AXIS2_PLACEMENT_3D('',#10466,#7060,#7061);
#5873=AXIS2_PLACEMENT_3D('',#10467,#7062,#7063);
#5874=AXIS2_PLACEMENT_3D('',#10468,#7064,#7065);
#5875=AXIS2_PLACEMENT_3D('',#10469,#7066,#7067);
#5876=AXIS2_PLACEMENT_3D('',#10470,#7068,#7069);
#5877=AXIS2_PLACEMENT_3D('',#10471,#7070,#7071);
#5878=AXIS2_PLACEMENT_3D('',#10472,#7072,#7073);
#5879=AXIS2_PLACEMENT_3D('',#10473,#7074,#7075);
#5880=AXIS2_PLACEMENT_3D('',#10474,#7076,#7077);
#5881=AXIS2_PLACEMENT_3D('',#10475,#7078,#7079);
#5882=AXIS2_PLACEMENT_3D('',#10476,#7080,#7081);
#5883=AXIS2_PLACEMENT_3D('',#10477,#7082,#7083);
#5884=AXIS2_PLACEMENT_3D('',#10478,#7084,#7085);
#5885=AXIS2_PLACEMENT_3D('',#10479,#7086,#7087);
#5886=AXIS2_PLACEMENT_3D('',#10480,#7088,#7089);
#5887=AXIS2_PLACEMENT_3D('',#10481,#7090,#7091);
#5888=AXIS2_PLACEMENT_3D('',#10482,#7092,#7093);
#5889=AXIS2_PLACEMENT_3D('',#10483,#7094,#7095);
#5890=AXIS2_PLACEMENT_3D('',#10484,#7096,#7097);
#5891=AXIS2_PLACEMENT_3D('',#10485,#7098,#7099);
#5892=AXIS2_PLACEMENT_3D('',#10486,#7100,#7101);
#5893=AXIS2_PLACEMENT_3D('',#10487,#7102,#7103);
#5894=AXIS2_PLACEMENT_3D('',#10488,#7104,#7105);
#5895=AXIS2_PLACEMENT_3D('',#10489,#7106,#7107);
#5896=AXIS2_PLACEMENT_3D('',#10490,#7108,#7109);
#5897=AXIS2_PLACEMENT_3D('',#10492,#7110,#7111);
#5898=AXIS2_PLACEMENT_3D('',#10494,#7112,#7113);
#5899=AXIS2_PLACEMENT_3D('',#10495,#7114,#7115);
#5900=AXIS2_PLACEMENT_3D('',#10497,#7116,#7117);
#5901=AXIS2_PLACEMENT_3D('',#10499,#7119,#7120);
#5902=AXIS2_PLACEMENT_3D('',#10501,#7121,#7122);
#5903=AXIS2_PLACEMENT_3D('',#10503,#7123,#7124);
#5904=AXIS2_PLACEMENT_3D('',#10504,#7125,#7126);
#5905=AXIS2_PLACEMENT_3D('',#10506,#7128,#7129);
#5906=AXIS2_PLACEMENT_3D('',#10509,#7131,#7132);
#5907=AXIS2_PLACEMENT_3D('',#10510,#7133,#7134);
#5908=AXIS2_PLACEMENT_3D('',#10511,#7135,#7136);
#5909=AXIS2_PLACEMENT_3D('',#10512,#7137,#7138);
#5910=AXIS2_PLACEMENT_3D('',#10513,#7139,#7140);
#5911=AXIS2_PLACEMENT_3D('',#10515,#7141,#7142);
#5912=AXIS2_PLACEMENT_3D('',#10518,#7144,#7145);
#5913=AXIS2_PLACEMENT_3D('',#10519,#7146,#7147);
#5914=AXIS2_PLACEMENT_3D('',#10521,#7148,#7149);
#5915=AXIS2_PLACEMENT_3D('',#10524,#7151,#7152);
#5916=AXIS2_PLACEMENT_3D('',#10525,#7153,#7154);
#5917=AXIS2_PLACEMENT_3D('',#10526,#7155,#7156);
#5918=AXIS2_PLACEMENT_3D('',#10527,#7157,#7158);
#5919=AXIS2_PLACEMENT_3D('',#10528,#7159,#7160);
#5920=AXIS2_PLACEMENT_3D('',#10532,#7162,#7163);
#5921=AXIS2_PLACEMENT_3D('',#10533,#7164,#7165);
#5922=AXIS2_PLACEMENT_3D('',#10550,#7166,#7167);
#5923=AXIS2_PLACEMENT_3D('',#10607,#7169,#7170);
#5924=AXIS2_PLACEMENT_3D('',#10609,#7172,#7173);
#5925=AXIS2_PLACEMENT_3D('',#10611,#7174,#7175);
#5926=AXIS2_PLACEMENT_3D('',#10614,#7177,#7178);
#5927=AXIS2_PLACEMENT_3D('',#10615,#7179,#7180);
#5928=AXIS2_PLACEMENT_3D('',#10617,#7181,#7182);
#5929=AXIS2_PLACEMENT_3D('',#10620,#7184,#7185);
#5930=AXIS2_PLACEMENT_3D('',#10621,#7186,#7187);
#5931=AXIS2_PLACEMENT_3D('',#10622,#7188,#7189);
#5932=AXIS2_PLACEMENT_3D('',#10623,#7190,#7191);
#5933=AXIS2_PLACEMENT_3D('',#10624,#7192,#7193);
#5934=AXIS2_PLACEMENT_3D('',#10626,#7194,#7195);
#5935=AXIS2_PLACEMENT_3D('',#10627,#7196,#7197);
#5936=AXIS2_PLACEMENT_3D('',#10636,#7202,#7203);
#5937=AXIS2_PLACEMENT_3D('',#10642,#7207,#7208);
#5938=AXIS2_PLACEMENT_3D('',#10648,#7212,#7213);
#5939=AXIS2_PLACEMENT_3D('',#10654,#7217,#7218);
#5940=AXIS2_PLACEMENT_3D('',#10660,#7222,#7223);
#5941=AXIS2_PLACEMENT_3D('',#10663,#7226,#7227);
#5942=AXIS2_PLACEMENT_3D('',#10664,#7228,#7229);
#5943=AXIS2_PLACEMENT_3D('',#10666,#7230,#7231);
#5944=AXIS2_PLACEMENT_3D('',#10667,#7232,#7233);
#5945=AXIS2_PLACEMENT_3D('',#10669,#7234,#7235);
#5946=AXIS2_PLACEMENT_3D('',#10671,#7237,#7238);
#5947=AXIS2_PLACEMENT_3D('',#10673,#7240,#7241);
#5948=AXIS2_PLACEMENT_3D('',#10674,#7242,#7243);
#5949=AXIS2_PLACEMENT_3D('',#10678,#7245,#7246);
#5950=AXIS2_PLACEMENT_3D('',#10679,#7247,#7248);
#5951=AXIS2_PLACEMENT_3D('',#10696,#7249,#7250);
#5952=AXIS2_PLACEMENT_3D('',#10737,#7252,#7253);
#5953=AXIS2_PLACEMENT_3D('',#10752,#7254,#7255);
#5954=AXIS2_PLACEMENT_3D('',#10754,#7257,#7258);
#5955=AXIS2_PLACEMENT_3D('',#10756,#7259,#7260);
#5956=AXIS2_PLACEMENT_3D('',#10759,#7262,#7263);
#5957=AXIS2_PLACEMENT_3D('',#10760,#7264,#7265);
#5958=AXIS2_PLACEMENT_3D('',#10762,#7266,#7267);
#5959=AXIS2_PLACEMENT_3D('',#10763,#7268,#7269);
#5960=AXIS2_PLACEMENT_3D('',#10765,#7270,#7271);
#5961=AXIS2_PLACEMENT_3D('',#10767,#7273,#7274);
#5962=AXIS2_PLACEMENT_3D('',#10776,#7279,#7280);
#5963=AXIS2_PLACEMENT_3D('',#10782,#7284,#7285);
#5964=AXIS2_PLACEMENT_3D('',#10788,#7289,#7290);
#5965=AXIS2_PLACEMENT_3D('',#10794,#7294,#7295);
#5966=AXIS2_PLACEMENT_3D('',#10800,#7299,#7300);
#5967=AXIS2_PLACEMENT_3D('',#10806,#7304,#7305);
#5968=AXIS2_PLACEMENT_3D('',#10812,#7309,#7310);
#5969=AXIS2_PLACEMENT_3D('',#10818,#7314,#7315);
#5970=AXIS2_PLACEMENT_3D('',#10824,#7319,#7320);
#5971=AXIS2_PLACEMENT_3D('',#10830,#7324,#7325);
#5972=AXIS2_PLACEMENT_3D('',#10836,#7329,#7330);
#5973=AXIS2_PLACEMENT_3D('',#10842,#7334,#7335);
#5974=AXIS2_PLACEMENT_3D('',#10848,#7339,#7340);
#5975=AXIS2_PLACEMENT_3D('',#10854,#7344,#7345);
#5976=AXIS2_PLACEMENT_3D('',#10860,#7349,#7350);
#5977=AXIS2_PLACEMENT_3D('',#10866,#7354,#7355);
#5978=AXIS2_PLACEMENT_3D('',#10872,#7359,#7360);
#5979=AXIS2_PLACEMENT_3D('',#10878,#7364,#7365);
#5980=AXIS2_PLACEMENT_3D('',#10884,#7369,#7370);
#5981=AXIS2_PLACEMENT_3D('',#10890,#7374,#7375);
#5982=AXIS2_PLACEMENT_3D('',#10896,#7379,#7380);
#5983=AXIS2_PLACEMENT_3D('',#10902,#7384,#7385);
#5984=AXIS2_PLACEMENT_3D('',#10908,#7389,#7390);
#5985=AXIS2_PLACEMENT_3D('',#10914,#7394,#7395);
#5986=AXIS2_PLACEMENT_3D('',#10920,#7399,#7400);
#5987=AXIS2_PLACEMENT_3D('',#10926,#7404,#7405);
#5988=AXIS2_PLACEMENT_3D('',#10932,#7409,#7410);
#5989=AXIS2_PLACEMENT_3D('',#10938,#7414,#7415);
#5990=AXIS2_PLACEMENT_3D('',#10944,#7419,#7420);
#5991=AXIS2_PLACEMENT_3D('',#10950,#7424,#7425);
#5992=AXIS2_PLACEMENT_3D('',#10956,#7429,#7430);
#5993=AXIS2_PLACEMENT_3D('',#10962,#7434,#7435);
#5994=AXIS2_PLACEMENT_3D('',#10968,#7439,#7440);
#5995=AXIS2_PLACEMENT_3D('',#10974,#7444,#7445);
#5996=AXIS2_PLACEMENT_3D('',#10980,#7449,#7450);
#5997=AXIS2_PLACEMENT_3D('',#10986,#7454,#7455);
#5998=AXIS2_PLACEMENT_3D('',#10992,#7459,#7460);
#5999=AXIS2_PLACEMENT_3D('',#10998,#7464,#7465);
#6000=AXIS2_PLACEMENT_3D('',#11004,#7469,#7470);
#6001=AXIS2_PLACEMENT_3D('',#11010,#7474,#7475);
#6002=AXIS2_PLACEMENT_3D('',#11016,#7479,#7480);
#6003=AXIS2_PLACEMENT_3D('',#11022,#7484,#7485);
#6004=AXIS2_PLACEMENT_3D('',#11028,#7489,#7490);
#6005=AXIS2_PLACEMENT_3D('',#11034,#7494,#7495);
#6006=AXIS2_PLACEMENT_3D('',#11040,#7499,#7500);
#6007=AXIS2_PLACEMENT_3D('',#11046,#7504,#7505);
#6008=AXIS2_PLACEMENT_3D('',#11052,#7509,#7510);
#6009=AXIS2_PLACEMENT_3D('',#11055,#7513,#7514);
#6010=AXIS2_PLACEMENT_3D('',#11056,#7515,#7516);
#6011=AXIS2_PLACEMENT_3D('',#11057,#7517,#7518);
#6012=AXIS2_PLACEMENT_3D('',#11058,#7519,#7520);
#6013=AXIS2_PLACEMENT_3D('',#11067,#7525,#7526);
#6014=AXIS2_PLACEMENT_3D('',#11073,#7530,#7531);
#6015=AXIS2_PLACEMENT_3D('',#11079,#7535,#7536);
#6016=AXIS2_PLACEMENT_3D('',#11085,#7540,#7541);
#6017=AXIS2_PLACEMENT_3D('',#11091,#7545,#7546);
#6018=AXIS2_PLACEMENT_3D('',#11094,#7549,#7550);
#6019=AXIS2_PLACEMENT_3D('',#11095,#7551,#7552);
#6020=AXIS2_PLACEMENT_3D('',#11097,#7553,#7554);
#6021=AXIS2_PLACEMENT_3D('',#11098,#7555,#7556);
#6022=AXIS2_PLACEMENT_3D('',#11100,#7557,#7558);
#6023=AXIS2_PLACEMENT_3D('',#11102,#7560,#7561);
#6024=AXIS2_PLACEMENT_3D('',#11104,#7562,#7563);
#6025=AXIS2_PLACEMENT_3D('',#11106,#7565,#7566);
#6026=AXIS2_PLACEMENT_3D('',#11108,#7567,#7568);
#6027=AXIS2_PLACEMENT_3D('',#11110,#7570,#7571);
#6028=AXIS2_PLACEMENT_3D('',#11111,#7572,#7573);
#6029=AXIS2_PLACEMENT_3D('',#11112,#7574,#7575);
#6030=AXIS2_PLACEMENT_3D('',#11113,#7576,#7577);
#6031=AXIS2_PLACEMENT_3D('',#11114,#7578,#7579);
#6032=AXIS2_PLACEMENT_3D('',#11115,#7580,#7581);
#6033=AXIS2_PLACEMENT_3D('',#11116,#7582,#7583);
#6034=AXIS2_PLACEMENT_3D('',#11117,#7584,#7585);
#6035=AXIS2_PLACEMENT_3D('',#11118,#7586,#7587);
#6036=AXIS2_PLACEMENT_3D('',#11119,#7588,#7589);
#6037=AXIS2_PLACEMENT_3D('',#11124,#7591,#7592);
#6038=AXIS2_PLACEMENT_3D('',#11127,#7594,#7595);
#6039=AXIS2_PLACEMENT_3D('',#11128,#7596,#7597);
#6040=AXIS2_PLACEMENT_3D('',#11138,#7602,#7603);
#6041=AXIS2_PLACEMENT_3D('',#11141,#7605,#7606);
#6042=AXIS2_PLACEMENT_3D('',#11142,#7607,#7608);
#6043=AXIS2_PLACEMENT_3D('',#11144,#7609,#7610);
#6044=AXIS2_PLACEMENT_3D('',#11148,#7612,#7613);
#6045=AXIS2_PLACEMENT_3D('',#11149,#7614,#7615);
#6046=AXIS2_PLACEMENT_3D('',#11150,#7616,#7617);
#6047=AXIS2_PLACEMENT_3D('',#11151,#7618,#7619);
#6048=AXIS2_PLACEMENT_3D('',#11153,#7621,#7622);
#6049=AXIS2_PLACEMENT_3D('',#11155,#7623,#7624);
#6050=AXIS2_PLACEMENT_3D('',#11162,#7629,#7630);
#6051=AXIS2_PLACEMENT_3D('',#11169,#7635,#7636);
#6052=AXIS2_PLACEMENT_3D('',#11171,#7638,#7639);
#6053=AXIS2_PLACEMENT_3D('',#11173,#7641,#7642);
#6054=AXIS2_PLACEMENT_3D('',#11174,#7643,#7644);
#6055=AXIS2_PLACEMENT_3D('',#11176,#7645,#7646);
#6056=AXIS2_PLACEMENT_3D('',#11178,#7648,#7649);
#6057=AXIS2_PLACEMENT_3D('',#11182,#7651,#7652);
#6058=AXIS2_PLACEMENT_3D('',#11184,#7654,#7655);
#6059=AXIS2_PLACEMENT_3D('',#11188,#7658,#7659);
#6060=AXIS2_PLACEMENT_3D('',#11192,#7662,#7663);
#6061=AXIS2_PLACEMENT_3D('',#11194,#7665,#7666);
#6062=AXIS2_PLACEMENT_3D('',#11195,#7667,#7668);
#6063=AXIS2_PLACEMENT_3D('',#11196,#7669,#7670);
#6064=AXIS2_PLACEMENT_3D('',#11197,#7671,#7672);
#6065=AXIS2_PLACEMENT_3D('',#11198,#7673,#7674);
#6066=DIRECTION('axis',(0.,0.,1.));
#6067=DIRECTION('refdir',(1.,0.,0.));
#6068=DIRECTION('axis',(0.,0.,1.));
#6069=DIRECTION('refdir',(1.,0.,0.));
#6070=DIRECTION('axis',(0.,0.,1.));
#6071=DIRECTION('refdir',(1.,0.,0.));
#6072=DIRECTION('center_axis',(0.,0.,1.));
#6073=DIRECTION('ref_axis',(1.,0.,0.));
#6074=DIRECTION('center_axis',(0.,0.,1.));
#6075=DIRECTION('ref_axis',(1.,0.,0.));
#6076=DIRECTION('',(0.,0.,1.));
#6077=DIRECTION('center_axis',(0.,0.,-1.));
#6078=DIRECTION('ref_axis',(1.,0.,0.));
#6079=DIRECTION('center_axis',(0.,0.,1.));
#6080=DIRECTION('ref_axis',(1.,0.,0.));
#6081=DIRECTION('center_axis',(0.,0.,1.));
#6082=DIRECTION('ref_axis',(1.,0.,0.));
#6083=DIRECTION('',(0.,0.,1.));
#6084=DIRECTION('center_axis',(0.,0.,-1.));
#6085=DIRECTION('ref_axis',(1.,0.,0.));
#6086=DIRECTION('center_axis',(0.,0.,1.));
#6087=DIRECTION('ref_axis',(1.,0.,0.));
#6088=DIRECTION('center_axis',(0.,0.,1.));
#6089=DIRECTION('ref_axis',(1.,0.,0.));
#6090=DIRECTION('',(0.,0.,1.));
#6091=DIRECTION('center_axis',(0.,0.,-1.));
#6092=DIRECTION('ref_axis',(1.,0.,0.));
#6093=DIRECTION('center_axis',(0.,0.,1.));
#6094=DIRECTION('ref_axis',(1.,0.,0.));
#6095=DIRECTION('center_axis',(0.,0.,1.));
#6096=DIRECTION('ref_axis',(1.,0.,0.));
#6097=DIRECTION('',(0.,0.,1.));
#6098=DIRECTION('center_axis',(0.,0.,-1.));
#6099=DIRECTION('ref_axis',(1.,0.,0.));
#6100=DIRECTION('center_axis',(0.,0.,1.));
#6101=DIRECTION('ref_axis',(1.,0.,0.));
#6102=DIRECTION('center_axis',(0.,0.,1.));
#6103=DIRECTION('ref_axis',(1.,0.,0.));
#6104=DIRECTION('',(0.,0.,1.));
#6105=DIRECTION('center_axis',(0.,0.,-1.));
#6106=DIRECTION('ref_axis',(1.,0.,0.));
#6107=DIRECTION('center_axis',(0.,0.,1.));
#6108=DIRECTION('ref_axis',(1.,0.,0.));
#6109=DIRECTION('center_axis',(0.,0.,1.));
#6110=DIRECTION('ref_axis',(1.,0.,0.));
#6111=DIRECTION('',(0.,0.,1.));
#6112=DIRECTION('center_axis',(0.,0.,-1.));
#6113=DIRECTION('ref_axis',(1.,0.,0.));
#6114=DIRECTION('center_axis',(0.,0.,1.));
#6115=DIRECTION('ref_axis',(1.,0.,0.));
#6116=DIRECTION('center_axis',(0.,0.,1.));
#6117=DIRECTION('ref_axis',(1.,0.,0.));
#6118=DIRECTION('',(0.,0.,1.));
#6119=DIRECTION('center_axis',(0.,0.,-1.));
#6120=DIRECTION('ref_axis',(1.,0.,0.));
#6121=DIRECTION('center_axis',(0.,1.,0.));
#6122=DIRECTION('ref_axis',(-1.,0.,0.));
#6123=DIRECTION('',(-1.,0.,0.));
#6124=DIRECTION('',(0.,0.,1.));
#6125=DIRECTION('',(-1.,0.,0.));
#6126=DIRECTION('',(0.,0.,1.));
#6127=DIRECTION('center_axis',(1.,0.,0.));
#6128=DIRECTION('ref_axis',(0.,1.,0.));
#6129=DIRECTION('',(0.,1.,0.));
#6130=DIRECTION('',(0.,1.,0.));
#6131=DIRECTION('',(0.,0.,1.));
#6132=DIRECTION('center_axis',(0.,-1.,0.));
#6133=DIRECTION('ref_axis',(1.,0.,0.));
#6134=DIRECTION('',(1.,0.,0.));
#6135=DIRECTION('',(1.,0.,0.));
#6136=DIRECTION('',(0.,0.,1.));
#6137=DIRECTION('center_axis',(-1.,0.,0.));
#6138=DIRECTION('ref_axis',(0.,-1.,0.));
#6139=DIRECTION('',(0.,-1.,0.));
#6140=DIRECTION('',(0.,-1.,0.));
#6141=DIRECTION('center_axis',(0.,0.,1.));
#6142=DIRECTION('ref_axis',(1.,0.,0.));
#6143=DIRECTION('center_axis',(0.,0.,1.));
#6144=DIRECTION('ref_axis',(1.,0.,0.));
#6145=DIRECTION('axis',(0.,0.,1.));
#6146=DIRECTION('refdir',(1.,0.,0.));
#6147=DIRECTION('center_axis',(0.,0.,1.));
#6148=DIRECTION('ref_axis',(1.,0.,0.));
#6149=DIRECTION('center_axis',(0.,0.,1.));
#6150=DIRECTION('ref_axis',(1.,0.,0.));
#6151=DIRECTION('',(0.,0.,1.));
#6152=DIRECTION('center_axis',(0.,0.,-1.));
#6153=DIRECTION('ref_axis',(1.,0.,0.));
#6154=DIRECTION('center_axis',(0.,0.,1.));
#6155=DIRECTION('ref_axis',(1.,0.,0.));
#6156=DIRECTION('center_axis',(0.,0.,1.));
#6157=DIRECTION('ref_axis',(1.,0.,0.));
#6158=DIRECTION('',(0.,0.,1.));
#6159=DIRECTION('center_axis',(0.,0.,-1.));
#6160=DIRECTION('ref_axis',(1.,0.,0.));
#6161=DIRECTION('center_axis',(0.,0.,1.));
#6162=DIRECTION('ref_axis',(1.,0.,0.));
#6163=DIRECTION('center_axis',(0.,0.,1.));
#6164=DIRECTION('ref_axis',(1.,0.,0.));
#6165=DIRECTION('',(0.,0.,1.));
#6166=DIRECTION('center_axis',(0.,0.,1.));
#6167=DIRECTION('ref_axis',(1.,0.,0.));
#6168=DIRECTION('center_axis',(0.,0.,1.));
#6169=DIRECTION('ref_axis',(1.,0.,0.));
#6170=DIRECTION('center_axis',(0.,0.,-1.));
#6171=DIRECTION('ref_axis',(1.,0.,0.));
#6172=DIRECTION('center_axis',(0.,0.,1.));
#6173=DIRECTION('ref_axis',(1.,0.,0.));
#6174=DIRECTION('',(0.,0.,1.));
#6175=DIRECTION('center_axis',(0.,0.,-1.));
#6176=DIRECTION('ref_axis',(1.,0.,0.));
#6177=DIRECTION('center_axis',(0.,0.,1.));
#6178=DIRECTION('ref_axis',(1.,0.,0.));
#6179=DIRECTION('center_axis',(0.,0.,1.));
#6180=DIRECTION('ref_axis',(1.,0.,0.));
#6181=DIRECTION('',(0.,0.,-1.));
#6182=DIRECTION('center_axis',(0.,0.,-1.));
#6183=DIRECTION('ref_axis',(1.,0.,0.));
#6184=DIRECTION('center_axis',(0.,0.,1.));
#6185=DIRECTION('ref_axis',(1.,0.,0.));
#6186=DIRECTION('center_axis',(0.,1.,0.));
#6187=DIRECTION('ref_axis',(-1.,0.,0.));
#6188=DIRECTION('',(-1.,0.,0.));
#6189=DIRECTION('',(0.,0.,1.));
#6190=DIRECTION('',(-1.,0.,0.));
#6191=DIRECTION('',(0.,0.,1.));
#6192=DIRECTION('center_axis',(1.,0.,0.));
#6193=DIRECTION('ref_axis',(0.,1.,0.));
#6194=DIRECTION('',(0.,1.,0.));
#6195=DIRECTION('',(0.,1.,0.));
#6196=DIRECTION('',(0.,0.,1.));
#6197=DIRECTION('center_axis',(0.,-1.,0.));
#6198=DIRECTION('ref_axis',(1.,0.,0.));
#6199=DIRECTION('',(1.,0.,0.));
#6200=DIRECTION('',(1.,0.,0.));
#6201=DIRECTION('',(0.,0.,1.));
#6202=DIRECTION('center_axis',(-1.,0.,0.));
#6203=DIRECTION('ref_axis',(0.,-1.,0.));
#6204=DIRECTION('',(0.,-1.,0.));
#6205=DIRECTION('',(0.,-1.,0.));
#6206=DIRECTION('center_axis',(0.,0.,1.));
#6207=DIRECTION('ref_axis',(1.,0.,0.));
#6208=DIRECTION('center_axis',(0.,0.,1.));
#6209=DIRECTION('ref_axis',(1.,0.,0.));
#6210=DIRECTION('axis',(0.,0.,1.));
#6211=DIRECTION('refdir',(1.,0.,0.));
#6212=DIRECTION('center_axis',(0.,0.,1.));
#6213=DIRECTION('ref_axis',(1.,0.,0.));
#6214=DIRECTION('center_axis',(0.,0.,1.));
#6215=DIRECTION('ref_axis',(1.,0.,0.));
#6216=DIRECTION('',(0.,0.,1.));
#6217=DIRECTION('center_axis',(0.,0.,-1.));
#6218=DIRECTION('ref_axis',(1.,0.,0.));
#6219=DIRECTION('center_axis',(0.,0.,1.));
#6220=DIRECTION('ref_axis',(1.,0.,0.));
#6221=DIRECTION('center_axis',(0.,0.,1.));
#6222=DIRECTION('ref_axis',(1.,0.,0.));
#6223=DIRECTION('center_axis',(0.,0.,1.));
#6224=DIRECTION('ref_axis',(1.,0.,0.));
#6225=DIRECTION('center_axis',(0.,0.,1.));
#6226=DIRECTION('ref_axis',(1.,0.,0.));
#6227=DIRECTION('center_axis',(0.,0.,1.));
#6228=DIRECTION('ref_axis',(1.,0.,0.));
#6229=DIRECTION('',(0.,0.,-1.));
#6230=DIRECTION('center_axis',(0.,0.,1.));
#6231=DIRECTION('ref_axis',(1.,0.,0.));
#6232=DIRECTION('center_axis',(0.,0.,1.));
#6233=DIRECTION('ref_axis',(1.,0.,0.));
#6234=DIRECTION('center_axis',(0.,0.,1.));
#6235=DIRECTION('ref_axis',(1.,0.,0.));
#6236=DIRECTION('center_axis',(0.,0.,1.));
#6237=DIRECTION('ref_axis',(1.,0.,0.));
#6238=DIRECTION('',(0.,0.,-1.));
#6239=DIRECTION('center_axis',(0.,0.,1.));
#6240=DIRECTION('ref_axis',(1.,0.,0.));
#6241=DIRECTION('axis',(0.,0.,1.));
#6242=DIRECTION('refdir',(1.,0.,0.));
#6243=DIRECTION('center_axis',(0.,0.,1.));
#6244=DIRECTION('ref_axis',(1.,0.,0.));
#6245=DIRECTION('center_axis',(0.,0.,-1.));
#6246=DIRECTION('ref_axis',(1.,0.,0.));
#6247=DIRECTION('',(0.,0.,-1.));
#6248=DIRECTION('center_axis',(0.,0.,-1.));
#6249=DIRECTION('ref_axis',(1.,0.,0.));
#6250=DIRECTION('center_axis',(0.,0.,1.));
#6251=DIRECTION('ref_axis',(1.,0.,0.));
#6252=DIRECTION('center_axis',(0.,0.,1.));
#6253=DIRECTION('ref_axis',(1.,0.,0.));
#6254=DIRECTION('',(0.,0.,-1.));
#6255=DIRECTION('center_axis',(0.,0.,1.));
#6256=DIRECTION('ref_axis',(1.,0.,0.));
#6257=DIRECTION('center_axis',(0.,0.,1.));
#6258=DIRECTION('ref_axis',(1.,0.,0.));
#6259=DIRECTION('center_axis',(0.,0.,1.));
#6260=DIRECTION('ref_axis',(1.,0.,0.));
#6261=DIRECTION('axis',(0.,0.,1.));
#6262=DIRECTION('refdir',(1.,0.,0.));
#6263=DIRECTION('center_axis',(0.,0.,1.));
#6264=DIRECTION('ref_axis',(1.,0.,0.));
#6265=DIRECTION('center_axis',(0.,0.,-1.));
#6266=DIRECTION('ref_axis',(1.,0.,0.));
#6267=DIRECTION('',(0.,0.,-1.));
#6268=DIRECTION('center_axis',(0.,0.,-1.));
#6269=DIRECTION('ref_axis',(1.,0.,0.));
#6270=DIRECTION('center_axis',(0.,0.,1.));
#6271=DIRECTION('ref_axis',(1.,0.,0.));
#6272=DIRECTION('center_axis',(0.,0.,1.));
#6273=DIRECTION('ref_axis',(1.,0.,0.));
#6274=DIRECTION('',(0.,0.,-1.));
#6275=DIRECTION('center_axis',(0.,0.,1.));
#6276=DIRECTION('ref_axis',(1.,0.,0.));
#6277=DIRECTION('center_axis',(0.,0.,1.));
#6278=DIRECTION('ref_axis',(1.,0.,0.));
#6279=DIRECTION('center_axis',(0.,0.,1.));
#6280=DIRECTION('ref_axis',(1.,0.,0.));
#6281=DIRECTION('axis',(0.,0.,1.));
#6282=DIRECTION('refdir',(1.,0.,0.));
#6283=DIRECTION('center_axis',(0.,0.,1.));
#6284=DIRECTION('ref_axis',(1.,0.,0.));
#6285=DIRECTION('center_axis',(0.,0.,-1.));
#6286=DIRECTION('ref_axis',(1.,0.,0.));
#6287=DIRECTION('',(0.,0.,-1.));
#6288=DIRECTION('center_axis',(0.,0.,-1.));
#6289=DIRECTION('ref_axis',(1.,0.,0.));
#6290=DIRECTION('center_axis',(0.,0.,1.));
#6291=DIRECTION('ref_axis',(1.,0.,0.));
#6292=DIRECTION('center_axis',(0.,0.,1.));
#6293=DIRECTION('ref_axis',(1.,0.,0.));
#6294=DIRECTION('',(0.,0.,-1.));
#6295=DIRECTION('center_axis',(0.,0.,1.));
#6296=DIRECTION('ref_axis',(1.,0.,0.));
#6297=DIRECTION('center_axis',(0.,0.,1.));
#6298=DIRECTION('ref_axis',(1.,0.,0.));
#6299=DIRECTION('center_axis',(0.,0.,1.));
#6300=DIRECTION('ref_axis',(1.,0.,0.));
#6301=DIRECTION('axis',(0.,0.,1.));
#6302=DIRECTION('refdir',(1.,0.,0.));
#6303=DIRECTION('center_axis',(0.,0.,1.));
#6304=DIRECTION('ref_axis',(1.,0.,0.));
#6305=DIRECTION('center_axis',(0.,0.,1.));
#6306=DIRECTION('ref_axis',(1.,0.,0.));
#6307=DIRECTION('',(0.,0.,1.));
#6308=DIRECTION('center_axis',(0.,0.,1.));
#6309=DIRECTION('ref_axis',(1.,0.,0.));
#6310=DIRECTION('center_axis',(0.,0.,1.));
#6311=DIRECTION('ref_axis',(1.,0.,0.));
#6312=DIRECTION('center_axis',(0.,0.,1.));
#6313=DIRECTION('ref_axis',(1.,0.,0.));
#6314=DIRECTION('center_axis',(0.,0.,1.));
#6315=DIRECTION('ref_axis',(1.,0.,0.));
#6316=DIRECTION('',(0.,0.,-1.));
#6317=DIRECTION('center_axis',(0.,0.,-1.));
#6318=DIRECTION('ref_axis',(1.,0.,0.));
#6319=DIRECTION('center_axis',(0.,0.,-1.));
#6320=DIRECTION('ref_axis',(1.,0.,0.));
#6321=DIRECTION('center_axis',(0.,0.,1.));
#6322=DIRECTION('ref_axis',(1.,0.,0.));
#6323=DIRECTION('center_axis',(0.,0.,1.));
#6324=DIRECTION('ref_axis',(1.,0.,0.));
#6325=DIRECTION('',(0.,-1.,0.));
#6326=DIRECTION('',(1.,0.,0.));
#6327=DIRECTION('',(1.,0.,0.));
#6328=DIRECTION('',(0.,1.,0.));
#6329=DIRECTION('',(-1.,0.,0.));
#6330=DIRECTION('center_axis',(0.,0.,1.));
#6331=DIRECTION('ref_axis',(1.,0.,0.));
#6332=DIRECTION('',(0.,-1.,0.));
#6333=DIRECTION('',(-1.,0.,0.));
#6334=DIRECTION('',(0.,1.,0.));
#6335=DIRECTION('center_axis',(0.,0.,1.));
#6336=DIRECTION('ref_axis',(1.,0.,0.));
#6337=DIRECTION('center_axis',(0.,0.,1.));
#6338=DIRECTION('ref_axis',(1.,0.,0.));
#6339=DIRECTION('',(0.,1.,0.));
#6340=DIRECTION('',(1.,0.,0.));
#6341=DIRECTION('center_axis',(0.,1.,0.));
#6342=DIRECTION('ref_axis',(-1.,0.,0.));
#6343=DIRECTION('',(0.,0.,1.));
#6344=DIRECTION('',(0.,0.,1.));
#6345=DIRECTION('center_axis',(1.,0.,0.));
#6346=DIRECTION('ref_axis',(0.,1.,0.));
#6347=DIRECTION('',(0.,0.,1.));
#6348=DIRECTION('center_axis',(0.,-1.,0.));
#6349=DIRECTION('ref_axis',(1.,0.,0.));
#6350=DIRECTION('',(0.,0.,1.));
#6351=DIRECTION('center_axis',(-1.,0.,0.));
#6352=DIRECTION('ref_axis',(0.,-1.,0.));
#6353=DIRECTION('center_axis',(0.,0.,1.));
#6354=DIRECTION('ref_axis',(1.,0.,0.));
#6355=DIRECTION('',(0.,0.,-1.));
#6356=DIRECTION('center_axis',(0.,0.,1.));
#6357=DIRECTION('ref_axis',(1.,0.,0.));
#6358=DIRECTION('center_axis',(0.,0.,1.));
#6359=DIRECTION('ref_axis',(1.,0.,0.));
#6360=DIRECTION('axis',(0.,0.,1.));
#6361=DIRECTION('refdir',(1.,0.,0.));
#6362=DIRECTION('center_axis',(1.,0.,0.));
#6363=DIRECTION('ref_axis',(0.,0.,-1.));
#6364=DIRECTION('',(1.,0.,0.));
#6365=DIRECTION('center_axis',(0.,0.,1.));
#6366=DIRECTION('ref_axis',(1.,0.,0.));
#6367=DIRECTION('center_axis',(0.,0.,1.));
#6368=DIRECTION('ref_axis',(1.,0.,0.));
#6369=DIRECTION('',(0.,0.,1.));
#6370=DIRECTION('center_axis',(0.,0.,-1.));
#6371=DIRECTION('ref_axis',(1.,0.,0.));
#6372=DIRECTION('center_axis',(0.,0.,1.));
#6373=DIRECTION('ref_axis',(1.,0.,0.));
#6374=DIRECTION('center_axis',(0.,0.,1.));
#6375=DIRECTION('ref_axis',(1.,0.,0.));
#6376=DIRECTION('center_axis',(0.,0.,1.));
#6377=DIRECTION('ref_axis',(1.,0.,0.));
#6378=DIRECTION('',(0.,0.,1.));
#6379=DIRECTION('center_axis',(0.,0.,-1.));
#6380=DIRECTION('ref_axis',(1.,0.,0.));
#6381=DIRECTION('center_axis',(0.,0.,1.));
#6382=DIRECTION('ref_axis',(1.,0.,0.));
#6383=DIRECTION('center_axis',(0.,0.,1.));
#6384=DIRECTION('ref_axis',(1.,0.,0.));
#6385=DIRECTION('center_axis',(0.,0.,1.));
#6386=DIRECTION('ref_axis',(1.,0.,0.));
#6387=DIRECTION('',(0.,0.,1.));
#6388=DIRECTION('center_axis',(0.,0.,-1.));
#6389=DIRECTION('ref_axis',(1.,0.,0.));
#6390=DIRECTION('center_axis',(0.,0.,1.));
#6391=DIRECTION('ref_axis',(1.,0.,0.));
#6392=DIRECTION('center_axis',(0.,0.,1.));
#6393=DIRECTION('ref_axis',(1.,0.,0.));
#6394=DIRECTION('center_axis',(0.,0.,1.));
#6395=DIRECTION('ref_axis',(1.,0.,0.));
#6396=DIRECTION('',(0.,0.,1.));
#6397=DIRECTION('center_axis',(0.,0.,-1.));
#6398=DIRECTION('ref_axis',(1.,0.,0.));
#6399=DIRECTION('center_axis',(0.,0.,1.));
#6400=DIRECTION('ref_axis',(1.,0.,0.));
#6401=DIRECTION('center_axis',(0.,0.,1.));
#6402=DIRECTION('ref_axis',(1.,0.,0.));
#6403=DIRECTION('center_axis',(0.,0.,1.));
#6404=DIRECTION('ref_axis',(1.,0.,0.));
#6405=DIRECTION('center_axis',(0.,0.,1.));
#6406=DIRECTION('ref_axis',(1.,0.,0.));
#6407=DIRECTION('center_axis',(0.,0.,1.));
#6408=DIRECTION('ref_axis',(1.,0.,0.));
#6409=DIRECTION('',(0.,0.,1.));
#6410=DIRECTION('center_axis',(0.,0.,1.));
#6411=DIRECTION('ref_axis',(1.,0.,0.));
#6412=DIRECTION('',(0.,0.,-1.));
#6413=DIRECTION('center_axis',(0.,0.,1.));
#6414=DIRECTION('ref_axis',(1.,0.,0.));
#6415=DIRECTION('',(0.,0.,-1.));
#6416=DIRECTION('center_axis',(0.,0.,1.));
#6417=DIRECTION('ref_axis',(1.,0.,0.));
#6418=DIRECTION('',(0.,0.,1.));
#6419=DIRECTION('center_axis',(0.,0.,1.));
#6420=DIRECTION('ref_axis',(1.,0.,0.));
#6421=DIRECTION('center_axis',(0.,0.,1.));
#6422=DIRECTION('ref_axis',(1.,0.,0.));
#6423=DIRECTION('center_axis',(0.,0.,1.));
#6424=DIRECTION('ref_axis',(1.,0.,0.));
#6425=DIRECTION('center_axis',(0.,0.,1.));
#6426=DIRECTION('ref_axis',(-0.707106781186548,-0.707106781186547,0.));
#6427=DIRECTION('',(0.,0.,-1.));
#6428=DIRECTION('center_axis',(0.,0.,1.));
#6429=DIRECTION('ref_axis',(1.,0.,0.));
#6430=DIRECTION('',(0.,0.,1.));
#6431=DIRECTION('center_axis',(0.,0.,1.));
#6432=DIRECTION('ref_axis',(1.,0.,0.));
#6433=DIRECTION('center_axis',(0.,0.,1.));
#6434=DIRECTION('ref_axis',(1.,0.,0.));
#6435=DIRECTION('center_axis',(0.,0.,1.));
#6436=DIRECTION('ref_axis',(1.,0.,0.));
#6437=DIRECTION('center_axis',(0.,0.,1.));
#6438=DIRECTION('ref_axis',(-0.707106781186547,0.707106781186548,0.));
#6439=DIRECTION('',(0.,0.,-1.));
#6440=DIRECTION('center_axis',(0.,0.,1.));
#6441=DIRECTION('ref_axis',(1.,0.,0.));
#6442=DIRECTION('',(0.,0.,1.));
#6443=DIRECTION('center_axis',(0.,0.,1.));
#6444=DIRECTION('ref_axis',(1.,0.,0.));
#6445=DIRECTION('center_axis',(0.,0.,1.));
#6446=DIRECTION('ref_axis',(1.,0.,0.));
#6447=DIRECTION('center_axis',(0.,0.,1.));
#6448=DIRECTION('ref_axis',(1.,0.,0.));
#6449=DIRECTION('center_axis',(0.,0.,1.));
#6450=DIRECTION('ref_axis',(1.,0.,0.));
#6451=DIRECTION('center_axis',(0.,0.,1.));
#6452=DIRECTION('ref_axis',(1.,0.,0.));
#6453=DIRECTION('',(0.,0.,-1.));
#6454=DIRECTION('center_axis',(0.,0.,1.));
#6455=DIRECTION('ref_axis',(1.,0.,0.));
#6456=DIRECTION('center_axis',(0.,0.,1.));
#6457=DIRECTION('ref_axis',(1.,0.,0.));
#6458=DIRECTION('center_axis',(0.,0.,1.));
#6459=DIRECTION('ref_axis',(1.,0.,0.));
#6460=DIRECTION('center_axis',(0.,0.,1.));
#6461=DIRECTION('ref_axis',(1.,0.,0.));
#6462=DIRECTION('center_axis',(0.,0.,1.));
#6463=DIRECTION('ref_axis',(1.,0.,0.));
#6464=DIRECTION('center_axis',(0.,0.,1.));
#6465=DIRECTION('ref_axis',(1.,0.,0.));
#6466=DIRECTION('center_axis',(0.,0.,1.));
#6467=DIRECTION('ref_axis',(1.,0.,0.));
#6468=DIRECTION('center_axis',(0.,0.,-1.));
#6469=DIRECTION('ref_axis',(1.,0.,0.));
#6470=DIRECTION('center_axis',(0.,0.,-1.));
#6471=DIRECTION('ref_axis',(1.,0.,0.));
#6472=DIRECTION('center_axis',(0.,0.,-1.));
#6473=DIRECTION('ref_axis',(1.,0.,0.));
#6474=DIRECTION('center_axis',(0.,0.,-1.));
#6475=DIRECTION('ref_axis',(1.,0.,0.));
#6476=DIRECTION('center_axis',(0.,0.,1.));
#6477=DIRECTION('ref_axis',(1.,0.,0.));
#6478=DIRECTION('center_axis',(0.,0.,1.));
#6479=DIRECTION('ref_axis',(1.,0.,0.));
#6480=DIRECTION('',(0.,0.,1.));
#6481=DIRECTION('center_axis',(0.,0.,1.));
#6482=DIRECTION('ref_axis',(1.,0.,0.));
#6483=DIRECTION('center_axis',(0.,0.,1.));
#6484=DIRECTION('ref_axis',(1.,0.,0.));
#6485=DIRECTION('',(0.,0.,1.));
#6486=DIRECTION('center_axis',(0.,0.,1.));
#6487=DIRECTION('ref_axis',(1.,0.,0.));
#6488=DIRECTION('center_axis',(0.,0.,1.));
#6489=DIRECTION('ref_axis',(1.,0.,0.));
#6490=DIRECTION('',(0.,0.,1.));
#6491=DIRECTION('center_axis',(0.,0.,1.));
#6492=DIRECTION('ref_axis',(1.,0.,0.));
#6493=DIRECTION('center_axis',(0.,0.,1.));
#6494=DIRECTION('ref_axis',(1.,0.,0.));
#6495=DIRECTION('',(0.,0.,1.));
#6496=DIRECTION('center_axis',(0.,0.,1.));
#6497=DIRECTION('ref_axis',(1.,0.,0.));
#6498=DIRECTION('center_axis',(0.,0.,1.));
#6499=DIRECTION('ref_axis',(1.,0.,0.));
#6500=DIRECTION('',(0.,0.,1.));
#6501=DIRECTION('center_axis',(0.,0.,-1.));
#6502=DIRECTION('ref_axis',(1.,0.,0.));
#6503=DIRECTION('center_axis',(0.,0.,1.));
#6504=DIRECTION('ref_axis',(1.,0.,0.));
#6505=DIRECTION('center_axis',(0.,0.,1.));
#6506=DIRECTION('ref_axis',(1.,0.,0.));
#6507=DIRECTION('center_axis',(0.,0.,1.));
#6508=DIRECTION('ref_axis',(1.,0.,0.));
#6509=DIRECTION('',(0.,0.,-1.));
#6510=DIRECTION('center_axis',(0.,0.,1.));
#6511=DIRECTION('ref_axis',(1.,0.,0.));
#6512=DIRECTION('center_axis',(0.,0.,1.));
#6513=DIRECTION('ref_axis',(1.,0.,0.));
#6514=DIRECTION('',(0.,0.,-1.));
#6515=DIRECTION('center_axis',(0.,0.,-1.));
#6516=DIRECTION('ref_axis',(1.,0.,0.));
#6517=DIRECTION('center_axis',(0.,0.,1.));
#6518=DIRECTION('ref_axis',(1.,0.,0.));
#6519=DIRECTION('center_axis',(0.,0.,1.));
#6520=DIRECTION('ref_axis',(1.,0.,0.));
#6521=DIRECTION('axis',(0.,0.,1.));
#6522=DIRECTION('refdir',(1.,0.,0.));
#6523=DIRECTION('center_axis',(0.,0.,1.));
#6524=DIRECTION('ref_axis',(1.,0.,0.));
#6525=DIRECTION('center_axis',(0.,0.,1.));
#6526=DIRECTION('ref_axis',(1.,0.,0.));
#6527=DIRECTION('',(0.,0.,1.));
#6528=DIRECTION('center_axis',(0.,0.,-1.));
#6529=DIRECTION('ref_axis',(1.,0.,0.));
#6530=DIRECTION('center_axis',(0.,0.,1.));
#6531=DIRECTION('ref_axis',(1.,0.,0.));
#6532=DIRECTION('center_axis',(0.,0.,1.));
#6533=DIRECTION('ref_axis',(1.,0.,0.));
#6534=DIRECTION('center_axis',(0.,0.,1.));
#6535=DIRECTION('ref_axis',(1.,0.,0.));
#6536=DIRECTION('center_axis',(0.,0.,1.));
#6537=DIRECTION('ref_axis',(1.,0.,0.));
#6538=DIRECTION('',(0.,0.,1.));
#6539=DIRECTION('center_axis',(0.,0.,-1.));
#6540=DIRECTION('ref_axis',(1.,0.,0.));
#6541=DIRECTION('center_axis',(0.,0.,1.));
#6542=DIRECTION('ref_axis',(1.,0.,0.));
#6543=DIRECTION('center_axis',(0.,0.,1.));
#6544=DIRECTION('ref_axis',(1.,0.,0.));
#6545=DIRECTION('center_axis',(0.,0.,1.));
#6546=DIRECTION('ref_axis',(1.,0.,0.));
#6547=DIRECTION('center_axis',(0.,0.,1.));
#6548=DIRECTION('ref_axis',(1.,0.,0.));
#6549=DIRECTION('',(0.,0.,1.));
#6550=DIRECTION('center_axis',(0.,0.,-1.));
#6551=DIRECTION('ref_axis',(1.,0.,0.));
#6552=DIRECTION('center_axis',(0.,0.,1.));
#6553=DIRECTION('ref_axis',(1.,0.,0.));
#6554=DIRECTION('center_axis',(0.,0.,1.));
#6555=DIRECTION('ref_axis',(1.,0.,0.));
#6556=DIRECTION('center_axis',(0.,0.,1.));
#6557=DIRECTION('ref_axis',(1.,0.,0.));
#6558=DIRECTION('center_axis',(0.,0.,1.));
#6559=DIRECTION('ref_axis',(1.,0.,0.));
#6560=DIRECTION('',(0.,0.,1.));
#6561=DIRECTION('center_axis',(0.,0.,-1.));
#6562=DIRECTION('ref_axis',(1.,0.,0.));
#6563=DIRECTION('center_axis',(0.,0.,1.));
#6564=DIRECTION('ref_axis',(1.,0.,0.));
#6565=DIRECTION('center_axis',(0.,0.,1.));
#6566=DIRECTION('ref_axis',(1.,0.,0.));
#6567=DIRECTION('center_axis',(0.,0.,1.));
#6568=DIRECTION('ref_axis',(1.,0.,0.));
#6569=DIRECTION('center_axis',(0.,0.,1.));
#6570=DIRECTION('ref_axis',(1.,0.,0.));
#6571=DIRECTION('',(0.,0.,1.));
#6572=DIRECTION('center_axis',(0.,0.,1.));
#6573=DIRECTION('ref_axis',(1.,0.,0.));
#6574=DIRECTION('center_axis',(0.,0.,1.));
#6575=DIRECTION('ref_axis',(1.,0.,0.));
#6576=DIRECTION('',(0.,0.,1.));
#6577=DIRECTION('center_axis',(0.,0.,1.));
#6578=DIRECTION('ref_axis',(1.,0.,0.));
#6579=DIRECTION('center_axis',(0.,0.,1.));
#6580=DIRECTION('ref_axis',(1.,0.,0.));
#6581=DIRECTION('',(0.,0.,1.));
#6582=DIRECTION('center_axis',(0.,0.,1.));
#6583=DIRECTION('ref_axis',(1.,0.,0.));
#6584=DIRECTION('center_axis',(0.,0.,1.));
#6585=DIRECTION('ref_axis',(1.,0.,0.));
#6586=DIRECTION('',(0.,0.,1.));
#6587=DIRECTION('center_axis',(0.,0.,1.));
#6588=DIRECTION('ref_axis',(1.,0.,0.));
#6589=DIRECTION('center_axis',(0.,0.,1.));
#6590=DIRECTION('ref_axis',(1.,0.,0.));
#6591=DIRECTION('',(0.,0.,-1.));
#6592=DIRECTION('center_axis',(0.,0.,1.));
#6593=DIRECTION('ref_axis',(1.,0.,0.));
#6594=DIRECTION('center_axis',(0.,0.,1.));
#6595=DIRECTION('ref_axis',(1.,0.,0.));
#6596=DIRECTION('center_axis',(0.,0.,-1.));
#6597=DIRECTION('ref_axis',(1.,0.,0.));
#6598=DIRECTION('center_axis',(0.,0.,1.));
#6599=DIRECTION('ref_axis',(1.,0.,0.));
#6600=DIRECTION('center_axis',(0.,0.,-1.));
#6601=DIRECTION('ref_axis',(1.,0.,0.));
#6602=DIRECTION('',(0.,0.,-1.));
#6603=DIRECTION('center_axis',(0.,0.,1.));
#6604=DIRECTION('ref_axis',(1.,0.,0.));
#6605=DIRECTION('center_axis',(0.,0.,1.));
#6606=DIRECTION('ref_axis',(1.,0.,0.));
#6607=DIRECTION('',(0.,0.,-1.));
#6608=DIRECTION('center_axis',(0.,0.,1.));
#6609=DIRECTION('ref_axis',(1.,0.,0.));
#6610=DIRECTION('center_axis',(0.,0.,1.));
#6611=DIRECTION('ref_axis',(1.,0.,0.));
#6612=DIRECTION('center_axis',(0.,0.,1.));
#6613=DIRECTION('ref_axis',(1.,0.,0.));
#6614=DIRECTION('axis',(0.,0.,1.));
#6615=DIRECTION('refdir',(1.,0.,0.));
#6616=DIRECTION('axis',(0.,0.,1.));
#6617=DIRECTION('refdir',(1.,0.,0.));
#6618=DIRECTION('center_axis',(0.,-1.,0.));
#6619=DIRECTION('ref_axis',(0.,0.,-1.));
#6620=DIRECTION('center_axis',(0.,-1.,0.));
#6621=DIRECTION('ref_axis',(1.,0.,0.));
#6622=DIRECTION('center_axis',(0.,-1.,0.));
#6623=DIRECTION('ref_axis',(1.,0.,0.));
#6624=DIRECTION('center_axis',(1.,0.,1.22464679914735E-16));
#6625=DIRECTION('ref_axis',(-1.22464679914735E-16,0.,1.));
#6626=DIRECTION('center_axis',(0.,1.,0.));
#6627=DIRECTION('ref_axis',(1.,0.,0.));
#6628=DIRECTION('center_axis',(0.,1.,0.));
#6629=DIRECTION('ref_axis',(1.,0.,0.));
#6630=DIRECTION('center_axis',(0.,-1.,0.));
#6631=DIRECTION('ref_axis',(1.,0.,0.));
#6632=DIRECTION('',(0.,1.,0.));
#6633=DIRECTION('center_axis',(0.,-1.,0.));
#6634=DIRECTION('ref_axis',(1.,0.,0.));
#6635=DIRECTION('center_axis',(0.,-1.,0.));
#6636=DIRECTION('ref_axis',(1.,0.,0.));
#6637=DIRECTION('center_axis',(0.,-1.,0.));
#6638=DIRECTION('ref_axis',(1.,0.,0.));
#6639=DIRECTION('',(0.,1.,0.));
#6640=DIRECTION('center_axis',(0.,-1.,0.));
#6641=DIRECTION('ref_axis',(1.,0.,0.));
#6642=DIRECTION('center_axis',(0.,1.,0.));
#6643=DIRECTION('ref_axis',(1.,0.,0.));
#6644=DIRECTION('',(-0.707106781186547,0.707106781186548,-8.65956056235493E-17));
#6645=DIRECTION('center_axis',(0.,-1.,0.));
#6646=DIRECTION('ref_axis',(1.,0.,0.));
#6647=DIRECTION('center_axis',(0.,1.,0.));
#6648=DIRECTION('ref_axis',(0.,0.,1.));
#6649=DIRECTION('center_axis',(0.,-1.,0.));
#6650=DIRECTION('ref_axis',(1.,0.,0.));
#6651=DIRECTION('center_axis',(0.,-1.,0.));
#6652=DIRECTION('ref_axis',(1.,0.,0.));
#6653=DIRECTION('',(0.,1.,0.));
#6654=DIRECTION('center_axis',(0.,-1.,0.));
#6655=DIRECTION('ref_axis',(0.,0.,-1.));
#6656=DIRECTION('center_axis',(0.,-1.,0.));
#6657=DIRECTION('ref_axis',(1.,0.,0.));
#6658=DIRECTION('center_axis',(0.,-1.,0.));
#6659=DIRECTION('ref_axis',(1.,0.,0.));
#6660=DIRECTION('',(0.707106781186547,0.707106781186548,8.65956056235493E-17));
#6661=DIRECTION('axis',(0.,0.,1.));
#6662=DIRECTION('refdir',(1.,0.,0.));
#6663=DIRECTION('center_axis',(0.,-1.,0.));
#6664=DIRECTION('ref_axis',(0.,0.,-1.));
#6665=DIRECTION('center_axis',(0.,-1.,0.));
#6666=DIRECTION('ref_axis',(1.,0.,0.));
#6667=DIRECTION('center_axis',(0.,-1.,0.));
#6668=DIRECTION('ref_axis',(1.,0.,0.));
#6669=DIRECTION('center_axis',(1.,0.,1.22464679914735E-16));
#6670=DIRECTION('ref_axis',(-1.22464679914735E-16,0.,1.));
#6671=DIRECTION('center_axis',(0.,1.,0.));
#6672=DIRECTION('ref_axis',(1.,0.,0.));
#6673=DIRECTION('center_axis',(0.,1.,0.));
#6674=DIRECTION('ref_axis',(1.,0.,0.));
#6675=DIRECTION('center_axis',(0.,-1.,0.));
#6676=DIRECTION('ref_axis',(1.,0.,0.));
#6677=DIRECTION('center_axis',(0.,-1.,0.));
#6678=DIRECTION('ref_axis',(1.,0.,0.));
#6679=DIRECTION('',(0.,1.,0.));
#6680=DIRECTION('center_axis',(0.,1.,0.));
#6681=DIRECTION('ref_axis',(0.,0.,1.));
#6682=DIRECTION('center_axis',(0.,-1.,0.));
#6683=DIRECTION('ref_axis',(1.,0.,0.));
#6684=DIRECTION('center_axis',(0.,-1.,0.));
#6685=DIRECTION('ref_axis',(1.,0.,0.));
#6686=DIRECTION('center_axis',(0.,-1.,0.));
#6687=DIRECTION('ref_axis',(1.,0.,0.));
#6688=DIRECTION('center_axis',(0.,-1.,0.));
#6689=DIRECTION('ref_axis',(1.,0.,0.));
#6690=DIRECTION('',(0.707106781186548,0.707106781186547,8.65956056235494E-17));
#6691=DIRECTION('center_axis',(0.,-1.,0.));
#6692=DIRECTION('ref_axis',(1.,0.,0.));
#6693=DIRECTION('center_axis',(0.,-1.,0.));
#6694=DIRECTION('ref_axis',(1.,0.,0.));
#6695=DIRECTION('',(0.,1.,0.));
#6696=DIRECTION('center_axis',(0.,1.,0.));
#6697=DIRECTION('ref_axis',(1.,0.,0.));
#6698=DIRECTION('center_axis',(0.,-1.,0.));
#6699=DIRECTION('ref_axis',(1.,0.,0.));
#6700=DIRECTION('',(-0.707106781186548,0.707106781186547,-8.65956056235494E-17));
#6701=DIRECTION('center_axis',(0.,-1.,0.));
#6702=DIRECTION('ref_axis',(0.,0.,-1.));
#6703=DIRECTION('center_axis',(0.,-1.,0.));
#6704=DIRECTION('ref_axis',(1.,0.,0.));
#6705=DIRECTION('',(0.,1.,0.));
#6706=DIRECTION('axis',(0.,0.,1.));
#6707=DIRECTION('refdir',(1.,0.,0.));
#6708=DIRECTION('center_axis',(0.,0.,1.));
#6709=DIRECTION('ref_axis',(1.,0.,0.));
#6710=DIRECTION('center_axis',(1.22464679914735E-16,-1.,0.));
#6711=DIRECTION('ref_axis',(-1.,-1.22464679914735E-16,0.));
#6712=DIRECTION('center_axis',(0.707106781186548,0.,0.707106781186548));
#6713=DIRECTION('ref_axis',(0.707106781186548,0.,-0.707106781186548));
#6714=DIRECTION('center_axis',(8.65956056235494E-17,-1.,-8.65956056235493E-17));
#6715=DIRECTION('ref_axis',(-0.707106781186547,-1.22464679914735E-16,0.707106781186547));
#6716=DIRECTION('center_axis',(1.,0.,0.));
#6717=DIRECTION('ref_axis',(6.12323399573676E-17,0.,-1.));
#6718=DIRECTION('center_axis',(7.49879891330929E-33,-1.,-1.22464679914735E-16));
#6719=DIRECTION('ref_axis',(-6.12323399573676E-17,-1.22464679914735E-16,
1.));
#6720=DIRECTION('center_axis',(0.707106781186548,0.,-0.707106781186548));
#6721=DIRECTION('ref_axis',(-0.707106781186548,0.,-0.707106781186548));
#6722=DIRECTION('center_axis',(-8.65956056235493E-17,-1.,-8.65956056235494E-17));
#6723=DIRECTION('ref_axis',(0.707106781186547,-1.22464679914735E-16,0.707106781186547));
#6724=DIRECTION('center_axis',(0.,0.,-1.));
#6725=DIRECTION('ref_axis',(-1.,0.,-1.22464679914735E-16));
#6726=DIRECTION('center_axis',(-1.22464679914735E-16,-1.,-1.49975978266186E-32));
#6727=DIRECTION('ref_axis',(1.,-1.22464679914735E-16,1.22464679914735E-16));
#6728=DIRECTION('center_axis',(-0.707106781186547,0.,-0.707106781186548));
#6729=DIRECTION('ref_axis',(-0.707106781186548,0.,0.707106781186547));
#6730=DIRECTION('center_axis',(-8.65956056235493E-17,-1.,8.65956056235493E-17));
#6731=DIRECTION('ref_axis',(0.707106781186548,-1.22464679914735E-16,-0.707106781186547));
#6732=DIRECTION('center_axis',(-1.,0.,0.));
#6733=DIRECTION('ref_axis',(-1.83697019872103E-16,0.,1.));
#6734=DIRECTION('center_axis',(-2.24963967399279E-32,-1.,1.22464679914735E-16));
#6735=DIRECTION('ref_axis',(1.83697019872103E-16,-1.22464679914735E-16,
-1.));
#6736=DIRECTION('center_axis',(-0.707106781186548,0.,0.707106781186548));
#6737=DIRECTION('ref_axis',(0.707106781186547,0.,0.707106781186548));
#6738=DIRECTION('center_axis',(8.65956056235493E-17,-1.,8.65956056235493E-17));
#6739=DIRECTION('ref_axis',(-0.707106781186547,-1.22464679914735E-16,-0.707106781186548));
#6740=DIRECTION('axis',(0.,0.,1.));
#6741=DIRECTION('refdir',(1.,0.,0.));
#6742=DIRECTION('center_axis',(0.,0.,1.));
#6743=DIRECTION('ref_axis',(1.,0.,0.));
#6744=DIRECTION('center_axis',(0.,-1.,0.));
#6745=DIRECTION('ref_axis',(0.,0.,-1.));
#6746=DIRECTION('center_axis',(0.,-1.,0.));
#6747=DIRECTION('ref_axis',(0.,0.,-1.));
#6748=DIRECTION('center_axis',(0.,1.,0.));
#6749=DIRECTION('ref_axis',(1.,0.,0.));
#6750=DIRECTION('center_axis',(0.,1.,0.));
#6751=DIRECTION('ref_axis',(1.,0.,0.));
#6752=DIRECTION('center_axis',(0.,1.,0.));
#6753=DIRECTION('ref_axis',(1.,0.,0.));
#6754=DIRECTION('center_axis',(0.,1.,0.));
#6755=DIRECTION('ref_axis',(1.,0.,0.));
#6756=DIRECTION('',(0.,-1.,0.));
#6757=DIRECTION('center_axis',(0.,-1.,0.));
#6758=DIRECTION('ref_axis',(1.,0.,0.));
#6759=DIRECTION('center_axis',(0.,1.,0.));
#6760=DIRECTION('ref_axis',(1.,0.,0.));
#6761=DIRECTION('center_axis',(0.,1.,0.));
#6762=DIRECTION('ref_axis',(1.,0.,0.));
#6763=DIRECTION('center_axis',(0.,1.,0.));
#6764=DIRECTION('ref_axis',(1.,0.,0.));
#6765=DIRECTION('center_axis',(0.,1.,0.));
#6766=DIRECTION('ref_axis',(1.,0.,0.));
#6767=DIRECTION('center_axis',(0.,1.,0.));
#6768=DIRECTION('ref_axis',(1.,0.,0.));
#6769=DIRECTION('center_axis',(0.,1.,0.));
#6770=DIRECTION('ref_axis',(1.,0.,0.));
#6771=DIRECTION('center_axis',(0.,-1.,0.));
#6772=DIRECTION('ref_axis',(1.,0.,0.));
#6773=DIRECTION('center_axis',(0.,-1.,0.));
#6774=DIRECTION('ref_axis',(0.,0.,-1.));
#6775=DIRECTION('center_axis',(6.12323399573677E-17,0.,1.));
#6776=DIRECTION('ref_axis',(1.,0.,0.));
#6777=DIRECTION('center_axis',(0.,-1.,0.));
#6778=DIRECTION('ref_axis',(0.,0.,-1.));
#6779=DIRECTION('center_axis',(0.,1.,0.));
#6780=DIRECTION('ref_axis',(1.,0.,0.));
#6781=DIRECTION('center_axis',(0.,-1.,0.));
#6782=DIRECTION('ref_axis',(1.,0.,0.));
#6783=DIRECTION('center_axis',(0.,-1.,0.));
#6784=DIRECTION('ref_axis',(0.,0.,-1.));
#6785=DIRECTION('center_axis',(0.,0.,1.));
#6786=DIRECTION('ref_axis',(1.,0.,0.));
#6787=DIRECTION('center_axis',(0.,-1.,0.));
#6788=DIRECTION('ref_axis',(0.,0.,-1.));
#6789=DIRECTION('center_axis',(0.,1.,0.));
#6790=DIRECTION('ref_axis',(1.,0.,0.));
#6791=DIRECTION('center_axis',(0.,-1.,0.));
#6792=DIRECTION('ref_axis',(1.,0.,0.));
#6793=DIRECTION('center_axis',(0.,-1.,0.));
#6794=DIRECTION('ref_axis',(0.,0.,-1.));
#6795=DIRECTION('center_axis',(0.,0.,1.));
#6796=DIRECTION('ref_axis',(1.,0.,0.));
#6797=DIRECTION('center_axis',(0.,-1.,0.));
#6798=DIRECTION('ref_axis',(0.,0.,-1.));
#6799=DIRECTION('center_axis',(0.,1.,0.));
#6800=DIRECTION('ref_axis',(1.,0.,0.));
#6801=DIRECTION('center_axis',(0.,-1.,0.));
#6802=DIRECTION('ref_axis',(1.,0.,0.));
#6803=DIRECTION('center_axis',(0.,-1.,0.));
#6804=DIRECTION('ref_axis',(0.,0.,-1.));
#6805=DIRECTION('center_axis',(0.,0.,1.));
#6806=DIRECTION('ref_axis',(1.,0.,0.));
#6807=DIRECTION('center_axis',(0.,-1.,0.));
#6808=DIRECTION('ref_axis',(0.,0.,-1.));
#6809=DIRECTION('center_axis',(0.,1.,0.));
#6810=DIRECTION('ref_axis',(1.,0.,0.));
#6811=DIRECTION('center_axis',(0.,-1.,0.));
#6812=DIRECTION('ref_axis',(1.,0.,0.));
#6813=DIRECTION('center_axis',(0.,-1.,0.));
#6814=DIRECTION('ref_axis',(0.,0.,-1.));
#6815=DIRECTION('center_axis',(6.12323399573676E-17,0.,1.));
#6816=DIRECTION('ref_axis',(1.,0.,0.));
#6817=DIRECTION('center_axis',(0.,-1.,0.));
#6818=DIRECTION('ref_axis',(0.,0.,-1.));
#6819=DIRECTION('center_axis',(0.,1.,0.));
#6820=DIRECTION('ref_axis',(1.,0.,0.));
#6821=DIRECTION('center_axis',(0.,-1.,0.));
#6822=DIRECTION('ref_axis',(1.,0.,0.));
#6823=DIRECTION('center_axis',(0.,-1.,0.));
#6824=DIRECTION('ref_axis',(0.,0.,-1.));
#6825=DIRECTION('center_axis',(0.,0.,1.));
#6826=DIRECTION('ref_axis',(1.,0.,0.));
#6827=DIRECTION('center_axis',(0.,-1.,0.));
#6828=DIRECTION('ref_axis',(0.,0.,-1.));
#6829=DIRECTION('center_axis',(0.,1.,0.));
#6830=DIRECTION('ref_axis',(1.,0.,0.));
#6831=DIRECTION('center_axis',(0.,1.,0.));
#6832=DIRECTION('ref_axis',(1.,0.,0.));
#6833=DIRECTION('',(0.,1.,0.));
#6834=DIRECTION('center_axis',(0.,-1.,0.));
#6835=DIRECTION('ref_axis',(1.,0.,0.));
#6836=DIRECTION('center_axis',(0.,-1.,0.));
#6837=DIRECTION('ref_axis',(1.,0.,0.));
#6838=DIRECTION('center_axis',(0.,1.,0.));
#6839=DIRECTION('ref_axis',(1.,0.,0.));
#6840=DIRECTION('center_axis',(0.,-1.,0.));
#6841=DIRECTION('ref_axis',(0.,0.,-1.));
#6842=DIRECTION('center_axis',(0.,0.,1.));
#6843=DIRECTION('ref_axis',(1.,0.,0.));
#6844=DIRECTION('center_axis',(0.,-1.,0.));
#6845=DIRECTION('ref_axis',(0.,0.,-1.));
#6846=DIRECTION('center_axis',(0.,-1.,0.));
#6847=DIRECTION('ref_axis',(-1.,0.,0.));
#6848=DIRECTION('center_axis',(0.,1.,0.));
#6849=DIRECTION('ref_axis',(1.,0.,0.));
#6850=DIRECTION('axis',(0.,0.,1.));
#6851=DIRECTION('refdir',(1.,0.,0.));
#6852=DIRECTION('center_axis',(0.,1.,0.));
#6853=DIRECTION('ref_axis',(0.,0.,1.));
#6854=DIRECTION('center_axis',(0.,-1.,0.));
#6855=DIRECTION('ref_axis',(1.,0.,0.));
#6856=DIRECTION('center_axis',(0.,-1.,0.));
#6857=DIRECTION('ref_axis',(1.,0.,0.));
#6858=DIRECTION('center_axis',(0.,-1.,0.));
#6859=DIRECTION('ref_axis',(1.,0.,0.));
#6860=DIRECTION('center_axis',(0.,-1.,0.));
#6861=DIRECTION('ref_axis',(1.,0.,0.));
#6862=DIRECTION('',(0.,1.,0.));
#6863=DIRECTION('center_axis',(0.,-1.,0.));
#6864=DIRECTION('ref_axis',(0.,0.,-1.));
#6865=DIRECTION('center_axis',(0.,-1.,0.));
#6866=DIRECTION('ref_axis',(1.,0.,0.));
#6867=DIRECTION('center_axis',(0.,-1.,0.));
#6868=DIRECTION('ref_axis',(1.,0.,0.));
#6869=DIRECTION('',(0.,1.,0.));
#6870=DIRECTION('center_axis',(0.,1.,0.));
#6871=DIRECTION('ref_axis',(0.,0.,1.));
#6872=DIRECTION('center_axis',(0.,-1.,0.));
#6873=DIRECTION('ref_axis',(1.,0.,0.));
#6874=DIRECTION('center_axis',(0.,-1.,0.));
#6875=DIRECTION('ref_axis',(1.,0.,0.));
#6876=DIRECTION('center_axis',(0.,-1.,0.));
#6877=DIRECTION('ref_axis',(1.,0.,0.));
#6878=DIRECTION('center_axis',(0.,-1.,0.));
#6879=DIRECTION('ref_axis',(1.,0.,0.));
#6880=DIRECTION('',(0.,1.,0.));
#6881=DIRECTION('center_axis',(0.,-1.,0.));
#6882=DIRECTION('ref_axis',(0.,0.,-1.));
#6883=DIRECTION('center_axis',(0.,-1.,0.));
#6884=DIRECTION('ref_axis',(1.,0.,0.));
#6885=DIRECTION('center_axis',(0.,-1.,0.));
#6886=DIRECTION('ref_axis',(1.,0.,0.));
#6887=DIRECTION('',(0.,1.,0.));
#6888=DIRECTION('',(0.,0.,1.));
#6889=DIRECTION('',(1.,0.,0.));
#6890=DIRECTION('',(0.,0.,1.));
#6891=DIRECTION('',(1.,0.,0.));
#6892=DIRECTION('',(0.,0.,1.));
#6893=DIRECTION('',(1.,0.,0.));
#6894=DIRECTION('',(0.,0.,1.));
#6895=DIRECTION('',(1.,0.,0.));
#6896=DIRECTION('',(0.,0.,1.));
#6897=DIRECTION('',(1.,0.,0.));
#6898=DIRECTION('axis',(0.,0.,1.));
#6899=DIRECTION('refdir',(1.,0.,0.));
#6900=DIRECTION('center_axis',(0.866025403784439,0.,-0.5));
#6901=DIRECTION('ref_axis',(0.5,0.,0.866025403784439));
#6902=DIRECTION('',(-0.5,0.,-0.866025403784439));
#6903=DIRECTION('',(0.,-1.,0.));
#6904=DIRECTION('',(0.5,0.,0.866025403784439));
#6905=DIRECTION('',(0.,-1.,0.));
#6906=DIRECTION('center_axis',(1.20185167898973E-16,0.,-1.));
#6907=DIRECTION('ref_axis',(1.,0.,1.20185167898973E-16));
#6908=DIRECTION('',(-1.,0.,-1.20185167898973E-16));
#6909=DIRECTION('',(0.,-1.,0.));
#6910=DIRECTION('',(1.,0.,1.20185167898973E-16));
#6911=DIRECTION('center_axis',(-0.866025403784439,0.,-0.5));
#6912=DIRECTION('ref_axis',(0.5,0.,-0.866025403784439));
#6913=DIRECTION('',(-0.5,0.,0.866025403784439));
#6914=DIRECTION('',(0.,-1.,0.));
#6915=DIRECTION('',(0.5,0.,-0.866025403784439));
#6916=DIRECTION('center_axis',(-0.866025403784439,0.,0.5));
#6917=DIRECTION('ref_axis',(-0.5,0.,-0.866025403784439));
#6918=DIRECTION('',(0.5,0.,0.866025403784439));
#6919=DIRECTION('',(0.,-1.,0.));
#6920=DIRECTION('',(-0.5,0.,-0.866025403784439));
#6921=DIRECTION('center_axis',(-2.40370335797945E-16,0.,1.));
#6922=DIRECTION('ref_axis',(-1.,0.,-2.40370335797945E-16));
#6923=DIRECTION('',(1.,0.,2.40370335797945E-16));
#6924=DIRECTION('',(0.,-1.,0.));
#6925=DIRECTION('',(-1.,0.,-2.40370335797945E-16));
#6926=DIRECTION('center_axis',(0.866025403784439,0.,0.5));
#6927=DIRECTION('ref_axis',(-0.5,0.,0.866025403784439));
#6928=DIRECTION('',(0.5,0.,-0.866025403784439));
#6929=DIRECTION('',(-0.5,0.,0.866025403784439));
#6930=DIRECTION('center_axis',(0.,1.,0.));
#6931=DIRECTION('ref_axis',(1.,0.,0.));
#6932=DIRECTION('center_axis',(0.,-1.,0.));
#6933=DIRECTION('ref_axis',(0.,0.,-1.));
#6934=DIRECTION('center_axis',(0.,1.,0.));
#6935=DIRECTION('ref_axis',(1.,0.,0.));
#6936=DIRECTION('center_axis',(0.,1.,0.));
#6937=DIRECTION('ref_axis',(1.,0.,0.));
#6938=DIRECTION('center_axis',(0.,1.,0.));
#6939=DIRECTION('ref_axis',(0.,0.,1.));
#6940=DIRECTION('center_axis',(0.,-1.,0.));
#6941=DIRECTION('ref_axis',(1.,0.,0.));
#6942=DIRECTION('center_axis',(0.,-1.,0.));
#6943=DIRECTION('ref_axis',(1.,0.,0.));
#6944=DIRECTION('center_axis',(0.,-1.,0.));
#6945=DIRECTION('ref_axis',(1.,0.,0.));
#6946=DIRECTION('',(0.707106781186548,0.707106781186547,8.65956056235493E-17));
#6947=DIRECTION('center_axis',(0.,-1.,0.));
#6948=DIRECTION('ref_axis',(1.,0.,0.));
#6949=DIRECTION('center_axis',(0.,-1.,0.));
#6950=DIRECTION('ref_axis',(1.,0.,0.));
#6951=DIRECTION('',(0.,1.,0.));
#6952=DIRECTION('center_axis',(0.,1.,0.));
#6953=DIRECTION('ref_axis',(1.,0.,0.));
#6954=DIRECTION('center_axis',(0.,-1.,0.));
#6955=DIRECTION('ref_axis',(1.,0.,0.));
#6956=DIRECTION('',(-0.707106781186547,0.707106781186548,-8.65956056235493E-17));
#6957=DIRECTION('center_axis',(0.,-1.,0.));
#6958=DIRECTION('ref_axis',(0.,0.,-1.));
#6959=DIRECTION('center_axis',(0.,-1.,0.));
#6960=DIRECTION('ref_axis',(1.,0.,0.));
#6961=DIRECTION('center_axis',(0.,1.,0.));
#6962=DIRECTION('ref_axis',(1.,0.,0.));
#6963=DIRECTION('center_axis',(0.,1.,0.));
#6964=DIRECTION('ref_axis',(1.,0.,0.));
#6965=DIRECTION('',(-0.447213595499958,0.894427190999916,-5.47678698264203E-17));
#6966=DIRECTION('center_axis',(0.,-1.,0.));
#6967=DIRECTION('ref_axis',(1.,0.,0.));
#6968=DIRECTION('',(0.,1.,0.));
#6969=DIRECTION('axis',(0.,0.,1.));
#6970=DIRECTION('refdir',(1.,0.,0.));
#6971=DIRECTION('center_axis',(0.866025403784439,0.,-0.5));
#6972=DIRECTION('ref_axis',(0.5,0.,0.866025403784439));
#6973=DIRECTION('',(-0.5,0.,-0.866025403784439));
#6974=DIRECTION('',(0.,-1.,0.));
#6975=DIRECTION('',(0.5,0.,0.866025403784439));
#6976=DIRECTION('',(0.,-1.,0.));
#6977=DIRECTION('center_axis',(1.60246890531964E-16,0.,-1.));
#6978=DIRECTION('ref_axis',(1.,0.,1.60246890531964E-16));
#6979=DIRECTION('',(-1.,0.,-1.60246890531964E-16));
#6980=DIRECTION('',(0.,-1.,0.));
#6981=DIRECTION('',(1.,0.,1.60246890531964E-16));
#6982=DIRECTION('center_axis',(-0.866025403784439,0.,-0.5));
#6983=DIRECTION('ref_axis',(0.5,0.,-0.866025403784439));
#6984=DIRECTION('',(-0.5,0.,0.866025403784439));
#6985=DIRECTION('',(0.,-1.,0.));
#6986=DIRECTION('',(0.5,0.,-0.866025403784439));
#6987=DIRECTION('center_axis',(-0.866025403784439,0.,0.5));
#6988=DIRECTION('ref_axis',(-0.5,0.,-0.866025403784439));
#6989=DIRECTION('',(0.5,0.,0.866025403784439));
#6990=DIRECTION('',(0.,-1.,0.));
#6991=DIRECTION('',(-0.5,0.,-0.866025403784439));
#6992=DIRECTION('center_axis',(-1.60246890531964E-16,0.,1.));
#6993=DIRECTION('ref_axis',(-1.,0.,-1.60246890531964E-16));
#6994=DIRECTION('',(1.,0.,1.60246890531964E-16));
#6995=DIRECTION('',(0.,-1.,0.));
#6996=DIRECTION('',(-1.,0.,-1.60246890531964E-16));
#6997=DIRECTION('center_axis',(0.866025403784439,0.,0.5));
#6998=DIRECTION('ref_axis',(-0.5,0.,0.866025403784439));
#6999=DIRECTION('',(0.5,0.,-0.866025403784439));
#7000=DIRECTION('',(-0.5,0.,0.866025403784439));
#7001=DIRECTION('center_axis',(0.,1.,0.));
#7002=DIRECTION('ref_axis',(1.,0.,0.));
#7003=DIRECTION('center_axis',(0.,-1.,0.));
#7004=DIRECTION('ref_axis',(0.,0.,-1.));
#7005=DIRECTION('center_axis',(0.,1.,0.));
#7006=DIRECTION('ref_axis',(1.,0.,0.));
#7007=DIRECTION('center_axis',(0.,1.,0.));
#7008=DIRECTION('ref_axis',(1.,0.,0.));
#7009=DIRECTION('center_axis',(0.,1.,0.));
#7010=DIRECTION('ref_axis',(0.,0.,1.));
#7011=DIRECTION('center_axis',(0.,-1.,0.));
#7012=DIRECTION('ref_axis',(1.,0.,0.));
#7013=DIRECTION('center_axis',(0.,-1.,0.));
#7014=DIRECTION('ref_axis',(1.,0.,0.));
#7015=DIRECTION('center_axis',(0.,-1.,0.));
#7016=DIRECTION('ref_axis',(1.,0.,0.));
#7017=DIRECTION('',(0.707106781186547,0.707106781186548,8.65956056235493E-17));
#7018=DIRECTION('center_axis',(0.,-1.,0.));
#7019=DIRECTION('ref_axis',(1.,0.,0.));
#7020=DIRECTION('center_axis',(0.,-1.,0.));
#7021=DIRECTION('ref_axis',(1.,0.,0.));
#7022=DIRECTION('',(0.,1.,0.));
#7023=DIRECTION('center_axis',(0.,1.,0.));
#7024=DIRECTION('ref_axis',(1.,0.,0.));
#7025=DIRECTION('center_axis',(0.,-1.,0.));
#7026=DIRECTION('ref_axis',(1.,0.,0.));
#7027=DIRECTION('',(-0.707106781186547,0.707106781186548,-8.65956056235493E-17));
#7028=DIRECTION('center_axis',(0.,-1.,0.));
#7029=DIRECTION('ref_axis',(0.,0.,-1.));
#7030=DIRECTION('center_axis',(0.,-1.,0.));
#7031=DIRECTION('ref_axis',(1.,0.,0.));
#7032=DIRECTION('center_axis',(0.,1.,0.));
#7033=DIRECTION('ref_axis',(1.,0.,0.));
#7034=DIRECTION('center_axis',(0.,1.,0.));
#7035=DIRECTION('ref_axis',(1.,0.,0.));
#7036=DIRECTION('',(-0.447213595499958,0.894427190999916,-5.47678698264203E-17));
#7037=DIRECTION('center_axis',(0.,-1.,0.));
#7038=DIRECTION('ref_axis',(1.,0.,0.));
#7039=DIRECTION('',(0.,1.,0.));
#7040=DIRECTION('axis',(0.,0.,1.));
#7041=DIRECTION('refdir',(1.,0.,0.));
#7042=DIRECTION('center_axis',(0.999998225160355,-0.00106218492982768,0.00155609746344814));
#7043=DIRECTION('ref_axis',(-0.00116547091797426,0.300191357997798,0.953878289018561));
#7044=DIRECTION('center_axis',(0.00155609740738298,-0.0010621849112801,
0.999998225160462));
#7045=DIRECTION('ref_axis',(-0.00155444353908754,0.999998225160461,0.0010646037811343));
#7046=DIRECTION('center_axis',(0.999998225160355,-0.00106218492982768,0.00155609746344814));
#7047=DIRECTION('ref_axis',(-0.00116547091797426,0.300191357997798,0.953878289018561));
#7048=DIRECTION('center_axis',(0.00155609740738298,-0.0010621849112801,
0.999998225160462));
#7049=DIRECTION('ref_axis',(-0.00155444353908754,0.999998225160461,0.0010646037811343));
#7050=DIRECTION('center_axis',(0.00155609740738298,-0.0010621849112801,
0.999998225160462));
#7051=DIRECTION('ref_axis',(-0.00155444353908754,0.999998225160461,0.0010646037811343));
#7052=DIRECTION('center_axis',(0.999998225160355,-0.00106218492982768,0.00155609746344814));
#7053=DIRECTION('ref_axis',(-0.00116547091797426,0.300191357997798,0.953878289018561));
#7054=DIRECTION('center_axis',(0.999998225160355,-0.00106218492982768,0.00155609746344814));
#7055=DIRECTION('ref_axis',(-0.00116547091797426,0.300191357997798,0.953878289018561));
#7056=DIRECTION('center_axis',(0.00155609740738298,-0.0010621849112801,
0.999998225160462));
#7057=DIRECTION('ref_axis',(-0.00155444353908754,0.999998225160462,0.0010646037811343));
#7058=DIRECTION('',(0.,0.,1.));
#7059=DIRECTION('',(1.,0.,0.));
#7060=DIRECTION('',(0.,0.,1.));
#7061=DIRECTION('',(1.,0.,0.));
#7062=DIRECTION('',(0.,0.,1.));
#7063=DIRECTION('',(1.,0.,0.));
#7064=DIRECTION('',(0.,0.,1.));
#7065=DIRECTION('',(1.,0.,0.));
#7066=DIRECTION('',(0.,0.,1.));
#7067=DIRECTION('',(1.,0.,0.));
#7068=DIRECTION('',(0.,0.,1.));
#7069=DIRECTION('',(1.,0.,0.));
#7070=DIRECTION('',(0.,0.,1.));
#7071=DIRECTION('',(1.,0.,0.));
#7072=DIRECTION('',(0.,0.,1.));
#7073=DIRECTION('',(1.,0.,0.));
#7074=DIRECTION('',(0.,0.,1.));
#7075=DIRECTION('',(1.,0.,0.));
#7076=DIRECTION('',(0.,-1.,2.22044604925031E-16));
#7077=DIRECTION('',(1.,0.,0.));
#7078=DIRECTION('',(0.,-1.,2.22044604925031E-16));
#7079=DIRECTION('',(1.,0.,0.));
#7080=DIRECTION('',(0.,-1.,2.22044604925031E-16));
#7081=DIRECTION('',(1.,0.,0.));
#7082=DIRECTION('',(0.,-1.,2.22044604925031E-16));
#7083=DIRECTION('',(1.,0.,0.));
#7084=DIRECTION('',(0.,-1.,2.22044604925031E-16));
#7085=DIRECTION('',(1.,0.,0.));
#7086=DIRECTION('',(0.,-1.,2.22044604925031E-16));
#7087=DIRECTION('',(1.,0.,0.));
#7088=DIRECTION('',(0.,-1.,2.22044604925031E-16));
#7089=DIRECTION('',(1.,0.,0.));
#7090=DIRECTION('',(0.,-1.,2.22044604925031E-16));
#7091=DIRECTION('',(1.,0.,0.));
#7092=DIRECTION('',(0.,-1.,2.22044604925031E-16));
#7093=DIRECTION('',(1.,0.,0.));
#7094=DIRECTION('',(0.,-1.,2.22044604925031E-16));
#7095=DIRECTION('',(1.,0.,0.));
#7096=DIRECTION('',(0.,-1.,2.22044604925031E-16));
#7097=DIRECTION('',(1.,0.,0.));
#7098=DIRECTION('',(0.,-1.,2.22044604925031E-16));
#7099=DIRECTION('',(1.,0.,0.));
#7100=DIRECTION('',(0.,1.,2.22044604925031E-16));
#7101=DIRECTION('',(1.,0.,0.));
#7102=DIRECTION('',(0.,-1.,2.22044604925031E-16));
#7103=DIRECTION('',(1.,0.,0.));
#7104=DIRECTION('axis',(0.,0.,1.));
#7105=DIRECTION('refdir',(1.,0.,0.));
#7106=DIRECTION('axis',(0.,0.,1.));
#7107=DIRECTION('refdir',(1.,0.,0.));
#7108=DIRECTION('center_axis',(0.,0.,1.));
#7109=DIRECTION('ref_axis',(1.,0.,0.));
#7110=DIRECTION('center_axis',(0.,0.,1.));
#7111=DIRECTION('ref_axis',(1.,0.,0.));
#7112=DIRECTION('center_axis',(0.,0.,1.));
#7113=DIRECTION('ref_axis',(1.,0.,0.));
#7114=DIRECTION('center_axis',(0.,0.,1.));
#7115=DIRECTION('ref_axis',(1.,0.,0.));
#7116=DIRECTION('center_axis',(0.,0.,1.));
#7117=DIRECTION('ref_axis',(1.,0.,0.));
#7118=DIRECTION('',(0.,0.,-1.));
#7119=DIRECTION('center_axis',(0.,0.,1.));
#7120=DIRECTION('ref_axis',(1.,0.,0.));
#7121=DIRECTION('center_axis',(0.,0.,1.));
#7122=DIRECTION('ref_axis',(1.,0.,0.));
#7123=DIRECTION('center_axis',(0.,0.,-1.));
#7124=DIRECTION('ref_axis',(1.,0.,0.));
#7125=DIRECTION('center_axis',(0.,0.,1.));
#7126=DIRECTION('ref_axis',(1.,0.,0.));
#7127=DIRECTION('',(0.,0.,-1.));
#7128=DIRECTION('center_axis',(0.,0.,1.));
#7129=DIRECTION('ref_axis',(1.,0.,0.));
#7130=DIRECTION('',(0.,0.,-1.));
#7131=DIRECTION('center_axis',(0.,0.,1.));
#7132=DIRECTION('ref_axis',(1.,0.,0.));
#7133=DIRECTION('center_axis',(0.,0.,1.));
#7134=DIRECTION('ref_axis',(1.,0.,0.));
#7135=DIRECTION('center_axis',(0.,0.,1.));
#7136=DIRECTION('ref_axis',(1.,0.,0.));
#7137=DIRECTION('axis',(0.,0.,1.));
#7138=DIRECTION('refdir',(1.,0.,0.));
#7139=DIRECTION('center_axis',(0.,0.,1.));
#7140=DIRECTION('ref_axis',(1.,0.,0.));
#7141=DIRECTION('center_axis',(0.,0.,-1.));
#7142=DIRECTION('ref_axis',(1.,0.,0.));
#7143=DIRECTION('',(0.,0.,-1.));
#7144=DIRECTION('center_axis',(0.,0.,-1.));
#7145=DIRECTION('ref_axis',(1.,0.,0.));
#7146=DIRECTION('center_axis',(0.,0.,1.));
#7147=DIRECTION('ref_axis',(1.,0.,0.));
#7148=DIRECTION('center_axis',(0.,0.,1.));
#7149=DIRECTION('ref_axis',(1.,0.,0.));
#7150=DIRECTION('',(0.,0.,-1.));
#7151=DIRECTION('center_axis',(0.,0.,1.));
#7152=DIRECTION('ref_axis',(1.,0.,0.));
#7153=DIRECTION('center_axis',(0.,0.,1.));
#7154=DIRECTION('ref_axis',(1.,0.,0.));
#7155=DIRECTION('center_axis',(0.,0.,1.));
#7156=DIRECTION('ref_axis',(1.,0.,0.));
#7157=DIRECTION('axis',(0.,0.,1.));
#7158=DIRECTION('refdir',(1.,0.,0.));
#7159=DIRECTION('center_axis',(1.,0.,0.));
#7160=DIRECTION('ref_axis',(0.,0.,-1.));
#7161=DIRECTION('',(0.,0.,1.));
#7162=DIRECTION('center_axis',(1.,0.,0.));
#7163=DIRECTION('ref_axis',(0.,0.,-1.));
#7164=DIRECTION('center_axis',(1.,0.,0.));
#7165=DIRECTION('ref_axis',(0.,0.,-1.));
#7166=DIRECTION('center_axis',(1.,0.,0.));
#7167=DIRECTION('ref_axis',(0.,0.,-1.));
#7168=DIRECTION('',(1.,0.,0.));
#7169=DIRECTION('center_axis',(1.,0.,0.));
#7170=DIRECTION('ref_axis',(0.,0.,-1.));
#7171=DIRECTION('',(0.,0.,-1.));
#7172=DIRECTION('center_axis',(0.,0.,1.));
#7173=DIRECTION('ref_axis',(1.,0.,0.));
#7174=DIRECTION('center_axis',(0.,0.,-1.));
#7175=DIRECTION('ref_axis',(1.,0.,0.));
#7176=DIRECTION('',(0.,0.,-1.));
#7177=DIRECTION('center_axis',(0.,0.,-1.));
#7178=DIRECTION('ref_axis',(1.,0.,0.));
#7179=DIRECTION('center_axis',(0.,0.,1.));
#7180=DIRECTION('ref_axis',(1.,0.,0.));
#7181=DIRECTION('center_axis',(0.,0.,1.));
#7182=DIRECTION('ref_axis',(1.,0.,0.));
#7183=DIRECTION('',(0.,0.,-1.));
#7184=DIRECTION('center_axis',(0.,0.,1.));
#7185=DIRECTION('ref_axis',(1.,0.,0.));
#7186=DIRECTION('center_axis',(0.,0.,1.));
#7187=DIRECTION('ref_axis',(1.,0.,0.));
#7188=DIRECTION('center_axis',(0.,0.,1.));
#7189=DIRECTION('ref_axis',(1.,0.,0.));
#7190=DIRECTION('axis',(0.,0.,1.));
#7191=DIRECTION('refdir',(1.,0.,0.));
#7192=DIRECTION('center_axis',(0.,1.,0.));
#7193=DIRECTION('ref_axis',(1.,0.,0.));
#7194=DIRECTION('center_axis',(0.,1.,0.));
#7195=DIRECTION('ref_axis',(1.,0.,0.));
#7196=DIRECTION('center_axis',(0.866025403784439,0.,-0.5));
#7197=DIRECTION('ref_axis',(0.5,0.,0.866025403784439));
#7198=DIRECTION('',(0.5,0.,0.866025403784439));
#7199=DIRECTION('',(0.,-1.,0.));
#7200=DIRECTION('',(0.5,0.,0.866025403784439));
#7201=DIRECTION('',(0.,-1.,0.));
#7202=DIRECTION('center_axis',(1.20185167898973E-16,0.,-1.));
#7203=DIRECTION('ref_axis',(1.,0.,1.20185167898973E-16));
#7204=DIRECTION('',(1.,0.,1.20185167898973E-16));
#7205=DIRECTION('',(0.,-1.,0.));
#7206=DIRECTION('',(1.,0.,1.20185167898973E-16));
#7207=DIRECTION('center_axis',(-0.866025403784439,0.,-0.5));
#7208=DIRECTION('ref_axis',(0.5,0.,-0.866025403784439));
#7209=DIRECTION('',(0.5,0.,-0.866025403784439));
#7210=DIRECTION('',(0.,-1.,0.));
#7211=DIRECTION('',(0.5,0.,-0.866025403784439));
#7212=DIRECTION('center_axis',(-0.866025403784439,0.,0.5));
#7213=DIRECTION('ref_axis',(-0.5,0.,-0.866025403784439));
#7214=DIRECTION('',(-0.5,0.,-0.866025403784439));
#7215=DIRECTION('',(0.,-1.,0.));
#7216=DIRECTION('',(-0.5,0.,-0.866025403784439));
#7217=DIRECTION('center_axis',(-2.40370335797945E-16,0.,1.));
#7218=DIRECTION('ref_axis',(-1.,0.,-2.40370335797945E-16));
#7219=DIRECTION('',(-1.,0.,-2.40370335797945E-16));
#7220=DIRECTION('',(0.,-1.,0.));
#7221=DIRECTION('',(-1.,0.,-2.40370335797945E-16));
#7222=DIRECTION('center_axis',(0.866025403784439,0.,0.5));
#7223=DIRECTION('ref_axis',(-0.5,0.,0.866025403784439));
#7224=DIRECTION('',(-0.5,0.,0.866025403784439));
#7225=DIRECTION('',(-0.5,0.,0.866025403784439));
#7226=DIRECTION('center_axis',(0.,-1.,0.));
#7227=DIRECTION('ref_axis',(0.,0.,-1.));
#7228=DIRECTION('center_axis',(0.,1.,0.));
#7229=DIRECTION('ref_axis',(0.,0.,1.));
#7230=DIRECTION('center_axis',(0.,-1.,0.));
#7231=DIRECTION('ref_axis',(1.,0.,0.));
#7232=DIRECTION('center_axis',(0.,-1.,0.));
#7233=DIRECTION('ref_axis',(1.,0.,0.));
#7234=DIRECTION('center_axis',(0.,-1.,0.));
#7235=DIRECTION('ref_axis',(1.,0.,0.));
#7236=DIRECTION('',(0.707106781186548,0.707106781186547,8.65956056235494E-17));
#7237=DIRECTION('center_axis',(0.,-1.,0.));
#7238=DIRECTION('ref_axis',(1.,0.,0.));
#7239=DIRECTION('',(0.,1.,0.));
#7240=DIRECTION('axis',(0.,0.,1.));
#7241=DIRECTION('refdir',(1.,0.,0.));
#7242=DIRECTION('center_axis',(0.,0.,1.));
#7243=DIRECTION('ref_axis',(1.,0.,0.));
#7244=DIRECTION('',(0.,1.,0.));
#7245=DIRECTION('center_axis',(0.,0.,1.));
#7246=DIRECTION('ref_axis',(1.,0.,0.));
#7247=DIRECTION('center_axis',(0.,0.,1.));
#7248=DIRECTION('ref_axis',(1.,0.,0.));
#7249=DIRECTION('center_axis',(0.,0.,1.));
#7250=DIRECTION('ref_axis',(1.,0.,0.));
#7251=DIRECTION('',(0.,0.,1.));
#7252=DIRECTION('center_axis',(0.,0.,1.));
#7253=DIRECTION('ref_axis',(1.,0.,0.));
#7254=DIRECTION('center_axis',(0.,0.,1.));
#7255=DIRECTION('ref_axis',(1.,0.,0.));
#7256=DIRECTION('',(0.,-1.,0.));
#7257=DIRECTION('center_axis',(0.,1.,0.));
#7258=DIRECTION('ref_axis',(1.,0.,0.));
#7259=DIRECTION('center_axis',(0.,1.,0.));
#7260=DIRECTION('ref_axis',(1.,0.,0.));
#7261=DIRECTION('',(0.,-1.,0.));
#7262=DIRECTION('center_axis',(0.,-1.,0.));
#7263=DIRECTION('ref_axis',(1.,0.,0.));
#7264=DIRECTION('center_axis',(0.,1.,0.));
#7265=DIRECTION('ref_axis',(1.,0.,0.));
#7266=DIRECTION('center_axis',(0.,-1.,0.));
#7267=DIRECTION('ref_axis',(1.,0.,0.));
#7268=DIRECTION('center_axis',(0.,1.,0.));
#7269=DIRECTION('ref_axis',(1.,0.,0.));
#7270=DIRECTION('center_axis',(0.,1.,0.));
#7271=DIRECTION('ref_axis',(1.,0.,0.));
#7272=DIRECTION('',(0.,1.,0.));
#7273=DIRECTION('center_axis',(0.015706233006771,0.,0.999876649514697));
#7274=DIRECTION('ref_axis',(0.999876649514697,0.,-0.015706233006771));
#7275=DIRECTION('',(-0.999876649514697,0.,0.015706233006771));
#7276=DIRECTION('',(0.,1.,0.));
#7277=DIRECTION('',(0.999876649514697,0.,-0.015706233006771));
#7278=DIRECTION('',(0.,1.,0.));
#7279=DIRECTION('center_axis',(0.957469564385932,0.,-0.288534284400681));
#7280=DIRECTION('ref_axis',(-0.288534284400681,0.,-0.957469564385932));
#7281=DIRECTION('',(0.288534284400681,0.,0.957469564385932));
#7282=DIRECTION('',(-0.288534284400681,0.,-0.957469564385932));
#7283=DIRECTION('',(0.,1.,0.));
#7284=DIRECTION('center_axis',(-0.243616063552747,0.,0.9698717510986));
#7285=DIRECTION('ref_axis',(0.9698717510986,0.,0.243616063552747));
#7286=DIRECTION('',(-0.9698717510986,0.,-0.243616063552747));
#7287=DIRECTION('',(0.9698717510986,0.,0.243616063552747));
#7288=DIRECTION('',(0.,1.,0.));
#7289=DIRECTION('center_axis',(0.999522748094039,0.,-0.0308913587033594));
#7290=DIRECTION('ref_axis',(-0.0308913587033594,0.,-0.999522748094039));
#7291=DIRECTION('',(0.0308913587033594,0.,0.999522748094039));
#7292=DIRECTION('',(-0.0308913587033594,0.,-0.999522748094039));
#7293=DIRECTION('',(0.,1.,0.));
#7294=DIRECTION('center_axis',(-0.486336327975727,0.,0.873771695633983));
#7295=DIRECTION('ref_axis',(0.873771695633983,0.,0.486336327975727));
#7296=DIRECTION('',(-0.873771695633983,0.,-0.486336327975727));
#7297=DIRECTION('',(0.873771695633983,0.,0.486336327975727));
#7298=DIRECTION('',(0.,1.,0.));
#7299=DIRECTION('center_axis',(0.973460108308978,0.,0.228856762039213));
#7300=DIRECTION('ref_axis',(0.228856762039213,0.,-0.973460108308978));
#7301=DIRECTION('',(-0.228856762039213,0.,0.973460108308978));
#7302=DIRECTION('',(0.228856762039213,0.,-0.973460108308978));
#7303=DIRECTION('',(0.,1.,0.));
#7304=DIRECTION('center_axis',(-0.695913575355945,0.,0.71812554308791));
#7305=DIRECTION('ref_axis',(0.71812554308791,0.,0.695913575355945));
#7306=DIRECTION('',(-0.71812554308791,0.,-0.695913575355945));
#7307=DIRECTION('',(0.71812554308791,0.,0.695913575355945));
#7308=DIRECTION('',(0.,1.,0.));
#7309=DIRECTION('center_axis',(0.881057770861552,0.,0.473008672652493));
#7310=DIRECTION('ref_axis',(0.473008672652493,0.,-0.881057770861552));
#7311=DIRECTION('',(-0.473008672652493,0.,0.881057770861552));
#7312=DIRECTION('',(0.473008672652493,0.,-0.881057770861552));
#7313=DIRECTION('',(0.,1.,0.));
#7314=DIRECTION('center_axis',(-0.858065462627213,0.,0.513540321538968));
#7315=DIRECTION('ref_axis',(0.513540321538968,0.,0.858065462627213));
#7316=DIRECTION('',(-0.513540321538968,0.,-0.858065462627213));
#7317=DIRECTION('',(0.513540321538968,0.,0.858065462627213));
#7318=DIRECTION('',(0.,1.,0.));
#7319=DIRECTION('center_axis',(0.728612802346719,0.,0.684925823908298));
#7320=DIRECTION('ref_axis',(0.684925823908298,0.,-0.728612802346719));
#7321=DIRECTION('',(-0.684925823908298,0.,0.728612802346719));
#7322=DIRECTION('',(0.684925823908298,0.,-0.728612802346719));
#7323=DIRECTION('',(0.,1.,0.));
#7324=DIRECTION('center_axis',(-0.96174160664066,0.,0.273958175742654));
#7325=DIRECTION('ref_axis',(0.273958175742654,0.,0.96174160664066));
#7326=DIRECTION('',(-0.273958175742654,0.,-0.96174160664066));
#7327=DIRECTION('',(0.273958175742654,0.,0.96174160664066));
#7328=DIRECTION('',(0.,1.,0.));
#7329=DIRECTION('center_axis',(0.526514075441545,0.,0.850166412158193));
#7330=DIRECTION('ref_axis',(0.850166412158193,0.,-0.526514075441545));
#7331=DIRECTION('',(-0.850166412158193,0.,0.526514075441545));
#7332=DIRECTION('',(0.850166412158193,0.,-0.526514075441545));
#7333=DIRECTION('',(0.,1.,0.));
#7334=DIRECTION('center_axis',(-0.999876649514698,0.,0.0157062330067685));
#7335=DIRECTION('ref_axis',(0.0157062330067685,0.,0.999876649514698));
#7336=DIRECTION('',(-0.0157062330067685,0.,-0.999876649514698));
#7337=DIRECTION('',(0.0157062330067685,0.,0.999876649514698));
#7338=DIRECTION('',(0.,1.,0.));
#7339=DIRECTION('center_axis',(0.288534284400681,0.,0.957469564385932));
#7340=DIRECTION('ref_axis',(0.957469564385932,0.,-0.288534284400681));
#7341=DIRECTION('',(-0.957469564385932,0.,0.288534284400681));
#7342=DIRECTION('',(0.957469564385932,0.,-0.288534284400681));
#7343=DIRECTION('',(0.,1.,0.));
#7344=DIRECTION('center_axis',(-0.969871751098599,0.,-0.243616063552749));
#7345=DIRECTION('ref_axis',(-0.243616063552749,0.,0.969871751098599));
#7346=DIRECTION('',(0.243616063552749,0.,-0.969871751098599));
#7347=DIRECTION('',(-0.243616063552749,0.,0.969871751098599));
#7348=DIRECTION('',(0.,1.,0.));
#7349=DIRECTION('center_axis',(0.0308913587033598,0.,0.999522748094039));
#7350=DIRECTION('ref_axis',(0.999522748094039,0.,-0.0308913587033598));
#7351=DIRECTION('',(-0.999522748094039,0.,0.0308913587033598));
#7352=DIRECTION('',(0.999522748094039,0.,-0.0308913587033598));
#7353=DIRECTION('',(0.,1.,0.));
#7354=DIRECTION('center_axis',(-0.873771695633983,0.,-0.486336327975728));
#7355=DIRECTION('ref_axis',(-0.486336327975728,0.,0.873771695633983));
#7356=DIRECTION('',(0.486336327975728,0.,-0.873771695633983));
#7357=DIRECTION('',(-0.486336327975728,0.,0.873771695633983));
#7358=DIRECTION('',(0.,1.,0.));
#7359=DIRECTION('center_axis',(-0.228856762039212,0.,0.973460108308978));
#7360=DIRECTION('ref_axis',(0.973460108308978,0.,0.228856762039212));
#7361=DIRECTION('',(-0.973460108308978,0.,-0.228856762039212));
#7362=DIRECTION('',(0.973460108308978,0.,0.228856762039212));
#7363=DIRECTION('',(0.,1.,0.));
#7364=DIRECTION('center_axis',(-0.718125543087911,0.,-0.695913575355944));
#7365=DIRECTION('ref_axis',(-0.695913575355944,0.,0.718125543087911));
#7366=DIRECTION('',(0.695913575355944,0.,-0.718125543087911));
#7367=DIRECTION('',(-0.695913575355944,0.,0.718125543087911));
#7368=DIRECTION('',(0.,1.,0.));
#7369=DIRECTION('center_axis',(-0.473008672652494,0.,0.881057770861551));
#7370=DIRECTION('ref_axis',(0.881057770861551,0.,0.473008672652494));
#7371=DIRECTION('',(-0.881057770861551,0.,-0.473008672652494));
#7372=DIRECTION('',(0.881057770861551,0.,0.473008672652494));
#7373=DIRECTION('',(0.,1.,0.));
#7374=DIRECTION('center_axis',(-0.513540321538967,0.,-0.858065462627214));
#7375=DIRECTION('ref_axis',(-0.858065462627214,0.,0.513540321538967));
#7376=DIRECTION('',(0.858065462627214,0.,-0.513540321538967));
#7377=DIRECTION('',(-0.858065462627214,0.,0.513540321538967));
#7378=DIRECTION('',(0.,1.,0.));
#7379=DIRECTION('center_axis',(-0.684925823908296,0.,0.728612802346721));
#7380=DIRECTION('ref_axis',(0.728612802346721,0.,0.684925823908296));
#7381=DIRECTION('',(-0.728612802346721,0.,-0.684925823908296));
#7382=DIRECTION('',(0.728612802346721,0.,0.684925823908296));
#7383=DIRECTION('',(0.,1.,0.));
#7384=DIRECTION('center_axis',(-0.273958175742656,0.,-0.961741606640659));
#7385=DIRECTION('ref_axis',(-0.961741606640659,0.,0.273958175742656));
#7386=DIRECTION('',(0.961741606640659,0.,-0.273958175742656));
#7387=DIRECTION('',(-0.961741606640659,0.,0.273958175742656));
#7388=DIRECTION('',(0.,1.,0.));
#7389=DIRECTION('center_axis',(-0.850166412158193,0.,0.526514075441546));
#7390=DIRECTION('ref_axis',(0.526514075441546,0.,0.850166412158193));
#7391=DIRECTION('',(-0.526514075441546,0.,-0.850166412158193));
#7392=DIRECTION('',(0.526514075441546,0.,0.850166412158193));
#7393=DIRECTION('',(0.,1.,0.));
#7394=DIRECTION('center_axis',(-0.0157062330067692,0.,-0.999876649514697));
#7395=DIRECTION('ref_axis',(-0.999876649514697,0.,0.0157062330067692));
#7396=DIRECTION('',(0.999876649514697,0.,-0.0157062330067692));
#7397=DIRECTION('',(-0.999876649514697,0.,0.0157062330067692));
#7398=DIRECTION('',(0.,1.,0.));
#7399=DIRECTION('center_axis',(-0.957469564385932,0.,0.288534284400681));
#7400=DIRECTION('ref_axis',(0.288534284400681,0.,0.957469564385932));
#7401=DIRECTION('',(-0.288534284400681,0.,-0.957469564385932));
#7402=DIRECTION('',(0.288534284400681,0.,0.957469564385932));
#7403=DIRECTION('',(0.,1.,0.));
#7404=DIRECTION('center_axis',(0.24361606355275,0.,-0.969871751098599));
#7405=DIRECTION('ref_axis',(-0.969871751098599,0.,-0.24361606355275));
#7406=DIRECTION('',(0.969871751098599,0.,0.24361606355275));
#7407=DIRECTION('',(-0.969871751098599,0.,-0.24361606355275));
#7408=DIRECTION('',(0.,1.,0.));
#7409=DIRECTION('center_axis',(-0.999522748094039,0.,0.0308913587033594));
#7410=DIRECTION('ref_axis',(0.0308913587033594,0.,0.999522748094039));
#7411=DIRECTION('',(-0.0308913587033594,0.,-0.999522748094039));
#7412=DIRECTION('',(0.0308913587033594,0.,0.999522748094039));
#7413=DIRECTION('',(0.,1.,0.));
#7414=DIRECTION('center_axis',(0.486336327975727,0.,-0.873771695633983));
#7415=DIRECTION('ref_axis',(-0.873771695633983,0.,-0.486336327975727));
#7416=DIRECTION('',(0.873771695633983,0.,0.486336327975727));
#7417=DIRECTION('',(-0.873771695633983,0.,-0.486336327975727));
#7418=DIRECTION('',(0.,1.,0.));
#7419=DIRECTION('center_axis',(-0.973460108308978,0.,-0.228856762039212));
#7420=DIRECTION('ref_axis',(-0.228856762039212,0.,0.973460108308978));
#7421=DIRECTION('',(0.228856762039212,0.,-0.973460108308978));
#7422=DIRECTION('',(-0.228856762039212,0.,0.973460108308978));
#7423=DIRECTION('',(0.,1.,0.));
#7424=DIRECTION('center_axis',(0.695913575355945,0.,-0.718125543087909));
#7425=DIRECTION('ref_axis',(-0.718125543087909,0.,-0.695913575355945));
#7426=DIRECTION('',(0.718125543087909,0.,0.695913575355945));
#7427=DIRECTION('',(-0.718125543087909,0.,-0.695913575355945));
#7428=DIRECTION('',(0.,1.,0.));
#7429=DIRECTION('center_axis',(-0.881057770861552,0.,-0.473008672652493));
#7430=DIRECTION('ref_axis',(-0.473008672652493,0.,0.881057770861552));
#7431=DIRECTION('',(0.473008672652493,0.,-0.881057770861552));
#7432=DIRECTION('',(-0.473008672652493,0.,0.881057770861552));
#7433=DIRECTION('',(0.,1.,0.));
#7434=DIRECTION('center_axis',(0.858065462627214,0.,-0.513540321538968));
#7435=DIRECTION('ref_axis',(-0.513540321538968,0.,-0.858065462627214));
#7436=DIRECTION('',(0.513540321538968,0.,0.858065462627214));
#7437=DIRECTION('',(-0.513540321538968,0.,-0.858065462627214));
#7438=DIRECTION('',(0.,1.,0.));
#7439=DIRECTION('center_axis',(-0.728612802346719,0.,-0.684925823908298));
#7440=DIRECTION('ref_axis',(-0.684925823908298,0.,0.728612802346719));
#7441=DIRECTION('',(0.684925823908298,0.,-0.728612802346719));
#7442=DIRECTION('',(-0.684925823908298,0.,0.728612802346719));
#7443=DIRECTION('',(0.,1.,0.));
#7444=DIRECTION('center_axis',(0.96174160664066,0.,-0.273958175742653));
#7445=DIRECTION('ref_axis',(-0.273958175742653,0.,-0.96174160664066));
#7446=DIRECTION('',(0.273958175742653,0.,0.96174160664066));
#7447=DIRECTION('',(-0.273958175742653,0.,-0.96174160664066));
#7448=DIRECTION('',(0.,1.,0.));
#7449=DIRECTION('center_axis',(-0.526514075441546,0.,-0.850166412158193));
#7450=DIRECTION('ref_axis',(-0.850166412158193,0.,0.526514075441546));
#7451=DIRECTION('',(0.850166412158193,0.,-0.526514075441546));
#7452=DIRECTION('',(-0.850166412158193,0.,0.526514075441546));
#7453=DIRECTION('',(0.,1.,0.));
#7454=DIRECTION('center_axis',(0.999876649514698,0.,-0.0157062330067686));
#7455=DIRECTION('ref_axis',(-0.0157062330067686,0.,-0.999876649514698));
#7456=DIRECTION('',(0.0157062330067686,0.,0.999876649514698));
#7457=DIRECTION('',(-0.0157062330067686,0.,-0.999876649514698));
#7458=DIRECTION('',(0.,1.,0.));
#7459=DIRECTION('center_axis',(-0.288534284400682,0.,-0.957469564385932));
#7460=DIRECTION('ref_axis',(-0.957469564385932,0.,0.288534284400682));
#7461=DIRECTION('',(0.957469564385932,0.,-0.288534284400682));
#7462=DIRECTION('',(-0.957469564385932,0.,0.288534284400682));
#7463=DIRECTION('',(0.,1.,0.));
#7464=DIRECTION('center_axis',(0.969871751098599,0.,0.24361606355275));
#7465=DIRECTION('ref_axis',(0.24361606355275,0.,-0.969871751098599));
#7466=DIRECTION('',(-0.24361606355275,0.,0.969871751098599));
#7467=DIRECTION('',(0.24361606355275,0.,-0.969871751098599));
#7468=DIRECTION('',(0.,1.,0.));
#7469=DIRECTION('center_axis',(-0.0308913587033594,0.,-0.999522748094039));
#7470=DIRECTION('ref_axis',(-0.999522748094039,0.,0.0308913587033594));
#7471=DIRECTION('',(0.999522748094039,0.,-0.0308913587033594));
#7472=DIRECTION('',(-0.999522748094039,0.,0.0308913587033594));
#7473=DIRECTION('',(0.,1.,0.));
#7474=DIRECTION('center_axis',(0.873771695633986,0.,0.486336327975723));
#7475=DIRECTION('ref_axis',(0.486336327975723,0.,-0.873771695633986));
#7476=DIRECTION('',(-0.486336327975723,0.,0.873771695633986));
#7477=DIRECTION('',(0.486336327975723,0.,-0.873771695633986));
#7478=DIRECTION('',(0.,1.,0.));
#7479=DIRECTION('center_axis',(0.228856762039213,0.,-0.973460108308978));
#7480=DIRECTION('ref_axis',(-0.973460108308978,0.,-0.228856762039213));
#7481=DIRECTION('',(0.973460108308978,0.,0.228856762039213));
#7482=DIRECTION('',(-0.973460108308978,0.,-0.228856762039213));
#7483=DIRECTION('',(0.,1.,0.));
#7484=DIRECTION('center_axis',(0.718125543087909,0.,0.695913575355946));
#7485=DIRECTION('ref_axis',(0.695913575355946,0.,-0.718125543087909));
#7486=DIRECTION('',(-0.695913575355946,0.,0.718125543087909));
#7487=DIRECTION('',(0.695913575355946,0.,-0.718125543087909));
#7488=DIRECTION('',(0.,1.,0.));
#7489=DIRECTION('center_axis',(0.473008672652493,0.,-0.881057770861552));
#7490=DIRECTION('ref_axis',(-0.881057770861552,0.,-0.473008672652493));
#7491=DIRECTION('',(0.881057770861552,0.,0.473008672652493));
#7492=DIRECTION('',(-0.881057770861552,0.,-0.473008672652493));
#7493=DIRECTION('',(0.,1.,0.));
#7494=DIRECTION('center_axis',(0.513540321538969,0.,0.858065462627213));
#7495=DIRECTION('ref_axis',(0.858065462627213,0.,-0.513540321538969));
#7496=DIRECTION('',(-0.858065462627213,0.,0.513540321538969));
#7497=DIRECTION('',(0.858065462627213,0.,-0.513540321538969));
#7498=DIRECTION('',(0.,1.,0.));
#7499=DIRECTION('center_axis',(0.684925823908296,0.,-0.728612802346721));
#7500=DIRECTION('ref_axis',(-0.728612802346721,0.,-0.684925823908296));
#7501=DIRECTION('',(0.728612802346721,0.,0.684925823908296));
#7502=DIRECTION('',(-0.728612802346721,0.,-0.684925823908296));
#7503=DIRECTION('',(0.,1.,0.));
#7504=DIRECTION('center_axis',(0.27395817574266,0.,0.961741606640658));
#7505=DIRECTION('ref_axis',(0.961741606640658,0.,-0.27395817574266));
#7506=DIRECTION('',(-0.961741606640658,0.,0.27395817574266));
#7507=DIRECTION('',(0.961741606640658,0.,-0.27395817574266));
#7508=DIRECTION('',(0.,1.,0.));
#7509=DIRECTION('center_axis',(0.850166412158193,0.,-0.526514075441546));
#7510=DIRECTION('ref_axis',(-0.526514075441546,0.,-0.850166412158193));
#7511=DIRECTION('',(0.526514075441546,0.,0.850166412158193));
#7512=DIRECTION('',(-0.526514075441546,0.,-0.850166412158193));
#7513=DIRECTION('center_axis',(0.,1.,0.));
#7514=DIRECTION('ref_axis',(0.,0.,1.));
#7515=DIRECTION('center_axis',(0.,1.,0.));
#7516=DIRECTION('ref_axis',(1.,0.,0.));
#7517=DIRECTION('axis',(0.,0.,1.));
#7518=DIRECTION('refdir',(1.,0.,0.));
#7519=DIRECTION('center_axis',(0.866025403784439,0.,-0.5));
#7520=DIRECTION('ref_axis',(0.5,0.,0.866025403784439));
#7521=DIRECTION('',(0.5,0.,0.866025403784439));
#7522=DIRECTION('',(0.,-1.,0.));
#7523=DIRECTION('',(0.5,0.,0.866025403784439));
#7524=DIRECTION('',(0.,-1.,0.));
#7525=DIRECTION('center_axis',(1.92296268638356E-16,0.,-1.));
#7526=DIRECTION('ref_axis',(1.,0.,1.92296268638356E-16));
#7527=DIRECTION('',(1.,0.,1.92296268638356E-16));
#7528=DIRECTION('',(0.,-1.,0.));
#7529=DIRECTION('',(1.,0.,1.92296268638356E-16));
#7530=DIRECTION('center_axis',(-0.866025403784439,0.,-0.5));
#7531=DIRECTION('ref_axis',(0.5,0.,-0.866025403784439));
#7532=DIRECTION('',(0.5,0.,-0.866025403784439));
#7533=DIRECTION('',(0.,-1.,0.));
#7534=DIRECTION('',(0.5,0.,-0.866025403784438));
#7535=DIRECTION('center_axis',(-0.866025403784439,0.,0.5));
#7536=DIRECTION('ref_axis',(-0.5,0.,-0.866025403784439));
#7537=DIRECTION('',(-0.5,0.,-0.866025403784439));
#7538=DIRECTION('',(0.,-1.,0.));
#7539=DIRECTION('',(-0.5,0.,-0.866025403784439));
#7540=DIRECTION('center_axis',(-1.92296268638356E-16,0.,1.));
#7541=DIRECTION('ref_axis',(-1.,0.,-1.92296268638356E-16));
#7542=DIRECTION('',(-1.,0.,-1.92296268638356E-16));
#7543=DIRECTION('',(0.,-1.,0.));
#7544=DIRECTION('',(-1.,0.,-1.92296268638356E-16));
#7545=DIRECTION('center_axis',(0.866025403784439,0.,0.5));
#7546=DIRECTION('ref_axis',(-0.5,0.,0.866025403784439));
#7547=DIRECTION('',(-0.5,0.,0.866025403784439));
#7548=DIRECTION('',(-0.5,0.,0.866025403784439));
#7549=DIRECTION('center_axis',(0.,-1.,0.));
#7550=DIRECTION('ref_axis',(0.,0.,-1.));
#7551=DIRECTION('center_axis',(0.,1.,0.));
#7552=DIRECTION('ref_axis',(0.,0.,1.));
#7553=DIRECTION('center_axis',(0.,-1.,0.));
#7554=DIRECTION('ref_axis',(1.,0.,0.));
#7555=DIRECTION('center_axis',(0.,-1.,0.));
#7556=DIRECTION('ref_axis',(1.,0.,0.));
#7557=DIRECTION('center_axis',(0.,-1.,0.));
#7558=DIRECTION('ref_axis',(1.,0.,0.));
#7559=DIRECTION('',(0.707106781186547,0.707106781186548,8.65956056235493E-17));
#7560=DIRECTION('center_axis',(0.,-1.,0.));
#7561=DIRECTION('ref_axis',(1.,0.,0.));
#7562=DIRECTION('center_axis',(0.,1.,0.));
#7563=DIRECTION('ref_axis',(1.,0.,0.));
#7564=DIRECTION('',(0.,1.,0.));
#7565=DIRECTION('center_axis',(0.,1.,0.));
#7566=DIRECTION('ref_axis',(1.,0.,0.));
#7567=DIRECTION('center_axis',(0.,-1.,0.));
#7568=DIRECTION('ref_axis',(1.,0.,0.));
#7569=DIRECTION('',(-0.707106781186547,0.707106781186548,-8.65956056235493E-17));
#7570=DIRECTION('center_axis',(0.,-1.,0.));
#7571=DIRECTION('ref_axis',(0.,0.,-1.));
#7572=DIRECTION('',(0.,0.,1.));
#7573=DIRECTION('',(1.,0.,0.));
#7574=DIRECTION('',(0.,0.,1.));
#7575=DIRECTION('',(1.,0.,0.));
#7576=DIRECTION('',(0.,0.,1.));
#7577=DIRECTION('',(1.,0.,0.));
#7578=DIRECTION('',(0.,0.,1.));
#7579=DIRECTION('',(2.22044604925031E-16,-1.,0.));
#7580=DIRECTION('',(0.,-1.,2.22044604925031E-16));
#7581=DIRECTION('',(1.,0.,0.));
#7582=DIRECTION('',(0.,0.,1.));
#7583=DIRECTION('',(-1.,1.22464679914735E-16,0.));
#7584=DIRECTION('axis',(0.,0.,1.));
#7585=DIRECTION('refdir',(1.,0.,0.));
#7586=DIRECTION('axis',(0.,0.,1.));
#7587=DIRECTION('refdir',(1.,0.,0.));
#7588=DIRECTION('center_axis',(0.,0.,1.));
#7589=DIRECTION('ref_axis',(1.,0.,0.));
#7590=DIRECTION('',(0.,0.,-1.));
#7591=DIRECTION('center_axis',(0.,0.,-1.));
#7592=DIRECTION('ref_axis',(1.,0.,0.));
#7593=DIRECTION('',(0.,0.,1.));
#7594=DIRECTION('center_axis',(0.,0.,1.));
#7595=DIRECTION('ref_axis',(1.,0.,0.));
#7596=DIRECTION('center_axis',(0.,2.22044604925031E-16,1.));
#7597=DIRECTION('ref_axis',(0.,-1.,2.22044604925031E-16));
#7598=DIRECTION('',(0.438202247191011,0.898876404494382,-1.99590656112388E-16));
#7599=DIRECTION('',(-0.615893007805892,0.78782980581837,-1.74933357981104E-16));
#7600=DIRECTION('',(-1.,0.,0.));
#7601=DIRECTION('',(0.50579161179386,-0.862655693448417,1.91548042638083E-16));
#7602=DIRECTION('center_axis',(0.,2.22044604925031E-16,1.));
#7603=DIRECTION('ref_axis',(1.,0.,0.));
#7604=DIRECTION('',(-0.438202247191011,-0.898876404494382,1.99590656112388E-16));
#7605=DIRECTION('center_axis',(0.,-2.22044604925031E-16,-1.));
#7606=DIRECTION('ref_axis',(1.,0.,0.));
#7607=DIRECTION('center_axis',(0.,0.,1.));
#7608=DIRECTION('ref_axis',(1.,0.,0.));
#7609=DIRECTION('center_axis',(0.,0.,1.));
#7610=DIRECTION('ref_axis',(1.,0.,0.));
#7611=DIRECTION('',(0.,0.,-1.));
#7612=DIRECTION('center_axis',(0.,0.,-1.));
#7613=DIRECTION('ref_axis',(1.,0.,0.));
#7614=DIRECTION('center_axis',(0.,0.,1.));
#7615=DIRECTION('ref_axis',(1.,0.,0.));
#7616=DIRECTION('center_axis',(0.,0.,1.));
#7617=DIRECTION('ref_axis',(1.,0.,0.));
#7618=DIRECTION('center_axis',(0.,0.,1.));
#7619=DIRECTION('ref_axis',(1.,0.,0.));
#7620=DIRECTION('',(-1.,0.,0.));
#7621=DIRECTION('center_axis',(0.,0.,1.));
#7622=DIRECTION('ref_axis',(1.,0.,0.));
#7623=DIRECTION('center_axis',(0.,2.22044604925031E-16,1.));
#7624=DIRECTION('ref_axis',(1.,0.,0.));
#7625=DIRECTION('',(-0.615893007805892,0.78782980581837,-1.74933357981104E-16));
#7626=DIRECTION('',(-0.438202247191011,-0.898876404494382,0.));
#7627=DIRECTION('',(-1.,0.,0.));
#7628=DIRECTION('',(0.438202247191011,0.898876404494382,0.));
#7629=DIRECTION('center_axis',(0.,1.,0.));
#7630=DIRECTION('ref_axis',(-1.,0.,0.));
#7631=DIRECTION('',(0.,0.,1.));
#7632=DIRECTION('',(-1.,0.,0.));
#7633=DIRECTION('',(-1.,0.,0.));
#7634=DIRECTION('',(0.,0.,1.));
#7635=DIRECTION('center_axis',(0.898876404494382,-0.438202247191011,0.));
#7636=DIRECTION('ref_axis',(0.438202247191011,0.898876404494382,0.));
#7637=DIRECTION('',(0.438202247191011,0.898876404494382,0.));
#7638=DIRECTION('center_axis',(-0.898876404494382,0.438202247191011,0.));
#7639=DIRECTION('ref_axis',(-0.438202247191011,-0.898876404494382,0.));
#7640=DIRECTION('',(-0.438202247191011,-0.898876404494382,0.));
#7641=DIRECTION('center_axis',(0.,0.,1.));
#7642=DIRECTION('ref_axis',(1.,0.,0.));
#7643=DIRECTION('center_axis',(0.,2.22044604925031E-16,1.));
#7644=DIRECTION('ref_axis',(1.,0.,0.));
#7645=DIRECTION('center_axis',(0.,2.22044604925031E-16,1.));
#7646=DIRECTION('ref_axis',(1.,0.,0.));
#7647=DIRECTION('',(0.,2.22044604925031E-16,1.));
#7648=DIRECTION('center_axis',(0.,2.22044604925031E-16,1.));
#7649=DIRECTION('ref_axis',(0.185131832090925,-0.982713694189034,2.18206273980622E-16));
#7650=DIRECTION('',(0.,2.22044604925031E-16,1.));
#7651=DIRECTION('center_axis',(0.,2.22044604925031E-16,1.));
#7652=DIRECTION('ref_axis',(1.,0.,0.));
#7653=DIRECTION('',(0.,-2.22044604925031E-16,-1.));
#7654=DIRECTION('center_axis',(-0.862655693448417,-0.50579161179386,1.12308298615162E-16));
#7655=DIRECTION('ref_axis',(0.50579161179386,-0.862655693448417,1.91548042638083E-16));
#7656=DIRECTION('',(0.,2.22044604925031E-16,1.));
#7657=DIRECTION('',(-0.50579161179386,0.862655693448417,-1.91548042638083E-16));
#7658=DIRECTION('center_axis',(0.,1.,-2.22044604925031E-16));
#7659=DIRECTION('ref_axis',(-1.,0.,0.));
#7660=DIRECTION('',(1.,0.,0.));
#7661=DIRECTION('',(0.,2.22044604925031E-16,1.));
#7662=DIRECTION('center_axis',(0.78782980581837,0.615893007805892,-1.36755719594349E-16));
#7663=DIRECTION('ref_axis',(-0.615893007805892,0.78782980581837,-1.74933357981104E-16));
#7664=DIRECTION('',(0.615893007805892,-0.78782980581837,1.74933357981104E-16));
#7665=DIRECTION('center_axis',(0.,2.22044604925031E-16,1.));
#7666=DIRECTION('ref_axis',(1.,0.,0.));
#7667=DIRECTION('',(0.,0.,1.));
#7668=DIRECTION('',(1.,0.,0.));
#7669=DIRECTION('',(0.,0.,1.));
#7670=DIRECTION('',(1.,0.,0.));
#7671=DIRECTION('',(0.,0.,1.));
#7672=DIRECTION('',(0.656840111913116,0.75402988493956,0.));
#7673=DIRECTION('',(6.12323385329428E-17,-6.12323400958851E-17,1.));
#7674=DIRECTION('',(0.999999999999999,1.80411241501588E-16,-6.12323385329429E-17));
#7675=CARTESIAN_POINT('',(0.,0.,0.));
#7676=CARTESIAN_POINT('',(0.,0.,0.));
#7677=CARTESIAN_POINT('',(0.,0.,0.));
#7678=CARTESIAN_POINT('Origin',(8.8,-2.47,-0.1));
#7679=CARTESIAN_POINT('',(8.575,-2.47,0.));
#7680=CARTESIAN_POINT('Origin',(8.8,-2.47,0.));
#7681=CARTESIAN_POINT('',(8.575,-2.47,1.));
#7682=CARTESIAN_POINT('',(8.575,-2.47,-0.1));
#7683=CARTESIAN_POINT('Origin',(8.8,-2.47,1.));
#7684=CARTESIAN_POINT('Origin',(7.9,-3.47,-0.1));
#7685=CARTESIAN_POINT('',(7.69,-3.47,0.));
#7686=CARTESIAN_POINT('Origin',(7.9,-3.47,0.));
#7687=CARTESIAN_POINT('',(7.69,-3.47,1.));
#7688=CARTESIAN_POINT('',(7.69,-3.47,-0.1));
#7689=CARTESIAN_POINT('Origin',(7.9,-3.47,1.));
#7690=CARTESIAN_POINT('Origin',(5.1,-3.47,-0.1));
#7691=CARTESIAN_POINT('',(4.89,-3.47,0.));
#7692=CARTESIAN_POINT('Origin',(5.1,-3.47,0.));
#7693=CARTESIAN_POINT('',(4.89,-3.47,1.));
#7694=CARTESIAN_POINT('',(4.89,-3.47,-0.1));
#7695=CARTESIAN_POINT('Origin',(5.1,-3.47,1.));
#7696=CARTESIAN_POINT('Origin',(1.76776695296637,-1.76776695296637,-0.1));
#7697=CARTESIAN_POINT('',(1.55776695296637,-1.76776695296637,0.));
#7698=CARTESIAN_POINT('Origin',(1.76776695296637,-1.76776695296637,0.));
#7699=CARTESIAN_POINT('',(1.55776695296637,-1.76776695296637,1.));
#7700=CARTESIAN_POINT('',(1.55776695296637,-1.76776695296637,-0.1));
#7701=CARTESIAN_POINT('Origin',(1.76776695296637,-1.76776695296637,1.));
#7702=CARTESIAN_POINT('Origin',(-1.76776695296637,-1.76776695296637,-0.1));
#7703=CARTESIAN_POINT('',(-1.97776695296637,-1.76776695296637,0.));
#7704=CARTESIAN_POINT('Origin',(-1.76776695296637,-1.76776695296637,0.));
#7705=CARTESIAN_POINT('',(-1.97776695296637,-1.76776695296637,1.));
#7706=CARTESIAN_POINT('',(-1.97776695296637,-1.76776695296637,-0.1));
#7707=CARTESIAN_POINT('Origin',(-1.76776695296637,-1.76776695296637,1.));
#7708=CARTESIAN_POINT('Origin',(-1.76776695296637,1.76776695296637,-0.1));
#7709=CARTESIAN_POINT('',(-1.97776695296637,1.76776695296637,0.));
#7710=CARTESIAN_POINT('Origin',(-1.76776695296637,1.76776695296637,0.));
#7711=CARTESIAN_POINT('',(-1.97776695296637,1.76776695296637,1.));
#7712=CARTESIAN_POINT('',(-1.97776695296637,1.76776695296637,-0.1));
#7713=CARTESIAN_POINT('Origin',(-1.76776695296637,1.76776695296637,1.));
#7714=CARTESIAN_POINT('Origin',(1.76776695296637,1.76776695296637,-0.1));
#7715=CARTESIAN_POINT('',(1.55776695296637,1.76776695296637,0.));
#7716=CARTESIAN_POINT('Origin',(1.76776695296637,1.76776695296637,0.));
#7717=CARTESIAN_POINT('',(1.55776695296637,1.76776695296637,1.));
#7718=CARTESIAN_POINT('',(1.55776695296637,1.76776695296637,-0.1));
#7719=CARTESIAN_POINT('Origin',(1.76776695296637,1.76776695296637,1.));
#7720=CARTESIAN_POINT('Origin',(9.5,5.,0.));
#7721=CARTESIAN_POINT('',(9.5,5.,0.));
#7722=CARTESIAN_POINT('',(-5.5,5.,0.));
#7723=CARTESIAN_POINT('',(9.5,5.,0.));
#7724=CARTESIAN_POINT('',(-5.5,5.,1.));
#7725=CARTESIAN_POINT('',(-5.5,5.,0.));
#7726=CARTESIAN_POINT('',(9.5,5.,1.));
#7727=CARTESIAN_POINT('',(9.5,5.,1.));
#7728=CARTESIAN_POINT('',(9.5,5.,0.));
#7729=CARTESIAN_POINT('Origin',(9.5,-5.,0.));
#7730=CARTESIAN_POINT('',(9.5,-5.,0.));
#7731=CARTESIAN_POINT('',(9.5,-5.,0.));
#7732=CARTESIAN_POINT('',(9.5,-5.,1.));
#7733=CARTESIAN_POINT('',(9.5,-5.,1.));
#7734=CARTESIAN_POINT('',(9.5,-5.,0.));
#7735=CARTESIAN_POINT('Origin',(-5.5,-5.,0.));
#7736=CARTESIAN_POINT('',(-5.5,-5.,0.));
#7737=CARTESIAN_POINT('',(-5.5,-5.,0.));
#7738=CARTESIAN_POINT('',(-5.5,-5.,1.));
#7739=CARTESIAN_POINT('',(-5.5,-5.,1.));
#7740=CARTESIAN_POINT('',(-5.5,-5.,0.));
#7741=CARTESIAN_POINT('Origin',(-5.5,5.,0.));
#7742=CARTESIAN_POINT('',(-5.5,5.,0.));
#7743=CARTESIAN_POINT('',(-5.5,5.,1.));
#7744=CARTESIAN_POINT('Origin',(2.,0.,1.));
#7745=CARTESIAN_POINT('Origin',(2.,0.,0.));
#7746=CARTESIAN_POINT('',(0.,0.,0.));
#7747=CARTESIAN_POINT('Origin',(7.9,-3.47,0.9));
#7748=CARTESIAN_POINT('',(7.625,-3.47,1.));
#7749=CARTESIAN_POINT('Origin',(7.9,-3.47,1.));
#7750=CARTESIAN_POINT('',(7.625,-3.47,1.8));
#7751=CARTESIAN_POINT('',(7.625,-3.47,0.9));
#7752=CARTESIAN_POINT('Origin',(7.9,-3.47,1.8));
#7753=CARTESIAN_POINT('Origin',(5.1,-3.47,0.9));
#7754=CARTESIAN_POINT('',(4.825,-3.47,1.));
#7755=CARTESIAN_POINT('Origin',(5.1,-3.47,1.));
#7756=CARTESIAN_POINT('',(4.825,-3.47,1.8));
#7757=CARTESIAN_POINT('',(4.825,-3.47,0.9));
#7758=CARTESIAN_POINT('Origin',(5.1,-3.47,1.8));
#7759=CARTESIAN_POINT('Origin',(6.5,-3.47,0.9));
#7760=CARTESIAN_POINT('',(5.975,-3.47,1.));
#7761=CARTESIAN_POINT('Origin',(6.5,-3.47,1.));
#7762=CARTESIAN_POINT('',(5.975,-3.47,1.8));
#7763=CARTESIAN_POINT('',(5.975,-3.47,0.9));
#7764=CARTESIAN_POINT('Origin',(6.5,-3.47,1.8));
#7765=CARTESIAN_POINT('Origin',(6.5,-3.47,1.8));
#7766=CARTESIAN_POINT('',(6.195,-3.47,1.8));
#7767=CARTESIAN_POINT('Origin',(6.5,-3.47,1.8));
#7768=CARTESIAN_POINT('Origin',(6.5,-3.47,0.9));
#7769=CARTESIAN_POINT('',(6.195,-3.47,4.6));
#7770=CARTESIAN_POINT('',(6.195,-3.47,0.9));
#7771=CARTESIAN_POINT('Origin',(6.5,-3.47,4.6));
#7772=CARTESIAN_POINT('Origin',(6.5,-3.47,1.8));
#7773=CARTESIAN_POINT('',(5.6,-3.47,4.6));
#7774=CARTESIAN_POINT('Origin',(6.5,-3.47,4.6));
#7775=CARTESIAN_POINT('',(5.6,-3.47,1.8));
#7776=CARTESIAN_POINT('',(5.6,-3.47,1.8));
#7777=CARTESIAN_POINT('Origin',(6.5,-3.47,1.8));
#7778=CARTESIAN_POINT('Origin',(6.5,-3.47,4.6));
#7779=CARTESIAN_POINT('Origin',(8.4,-2.27,1.));
#7780=CARTESIAN_POINT('',(8.4,-2.27,1.));
#7781=CARTESIAN_POINT('',(4.6,-2.27,1.));
#7782=CARTESIAN_POINT('',(8.4,-2.27,1.));
#7783=CARTESIAN_POINT('',(4.6,-2.27,1.8));
#7784=CARTESIAN_POINT('',(4.6,-2.27,1.));
#7785=CARTESIAN_POINT('',(8.4,-2.27,1.8));
#7786=CARTESIAN_POINT('',(8.4,-2.27,1.8));
#7787=CARTESIAN_POINT('',(8.4,-2.27,1.));
#7788=CARTESIAN_POINT('Origin',(8.4,-4.67,1.));
#7789=CARTESIAN_POINT('',(8.4,-4.67,1.));
#7790=CARTESIAN_POINT('',(8.4,-4.67,1.));
#7791=CARTESIAN_POINT('',(8.4,-4.67,1.8));
#7792=CARTESIAN_POINT('',(8.4,-4.67,1.8));
#7793=CARTESIAN_POINT('',(8.4,-4.67,1.));
#7794=CARTESIAN_POINT('Origin',(4.6,-4.67,1.));
#7795=CARTESIAN_POINT('',(4.6,-4.67,1.));
#7796=CARTESIAN_POINT('',(4.6,-4.67,1.));
#7797=CARTESIAN_POINT('',(4.6,-4.67,1.8));
#7798=CARTESIAN_POINT('',(4.6,-4.67,1.8));
#7799=CARTESIAN_POINT('',(4.6,-4.67,1.));
#7800=CARTESIAN_POINT('Origin',(4.6,-2.27,1.));
#7801=CARTESIAN_POINT('',(4.6,-2.27,1.));
#7802=CARTESIAN_POINT('',(4.6,-2.27,1.8));
#7803=CARTESIAN_POINT('Origin',(6.5,-3.47,1.8));
#7804=CARTESIAN_POINT('Origin',(6.5,-3.47,1.));
#7805=CARTESIAN_POINT('',(0.,0.,0.));
#7806=CARTESIAN_POINT('Origin',(6.5,-3.47,5.5));
#7807=CARTESIAN_POINT('',(6.335,-3.47,5.5));
#7808=CARTESIAN_POINT('Origin',(6.5,-3.47,5.5));
#7809=CARTESIAN_POINT('',(6.335,-3.47,6.64));
#7810=CARTESIAN_POINT('',(6.335,-3.47,5.5));
#7811=CARTESIAN_POINT('Origin',(6.5,-3.47,6.64));
#7812=CARTESIAN_POINT('Origin',(6.5,-3.47,5.5));
#7813=CARTESIAN_POINT('Origin',(6.5,-3.47,1.8));
#7814=CARTESIAN_POINT('',(6.,-3.47,1.8));
#7815=CARTESIAN_POINT('Origin',(6.5,-3.47,1.8));
#7816=CARTESIAN_POINT('',(6.2,-3.47,1.8));
#7817=CARTESIAN_POINT('Origin',(6.5,-3.47,1.8));
#7818=CARTESIAN_POINT('Origin',(6.5,-3.47,1.6));
#7819=CARTESIAN_POINT('',(6.,-3.47,1.6));
#7820=CARTESIAN_POINT('',(6.,-3.47,1.6));
#7821=CARTESIAN_POINT('Origin',(6.5,-3.47,1.6));
#7822=CARTESIAN_POINT('Origin',(6.5,-3.47,1.6));
#7823=CARTESIAN_POINT('Origin',(6.5,-3.47,1.8));
#7824=CARTESIAN_POINT('',(6.2,-3.47,6.64));
#7825=CARTESIAN_POINT('Origin',(6.5,-3.47,6.64));
#7826=CARTESIAN_POINT('',(6.2,-3.47,1.8));
#7827=CARTESIAN_POINT('Origin',(6.5,-3.47,6.64));
#7828=CARTESIAN_POINT('',(0.,0.,0.));
#7829=CARTESIAN_POINT('Origin',(6.5,-3.47,4.6));
#7830=CARTESIAN_POINT('',(6.19,-3.47,4.8));
#7831=CARTESIAN_POINT('Origin',(6.5,-3.47,4.8));
#7832=CARTESIAN_POINT('',(6.19,-3.47,4.6));
#7833=CARTESIAN_POINT('',(6.19,-3.47,4.6));
#7834=CARTESIAN_POINT('Origin',(6.5,-3.47,4.6));
#7835=CARTESIAN_POINT('Origin',(6.5,-3.47,4.6));
#7836=CARTESIAN_POINT('',(6.,-3.47,4.8));
#7837=CARTESIAN_POINT('Origin',(6.5,-3.47,4.8));
#7838=CARTESIAN_POINT('',(6.,-3.47,4.6));
#7839=CARTESIAN_POINT('',(6.,-3.47,4.6));
#7840=CARTESIAN_POINT('Origin',(6.5,-3.47,4.6));
#7841=CARTESIAN_POINT('Origin',(6.5,-3.47,4.8));
#7842=CARTESIAN_POINT('Origin',(6.5,-3.47,4.6));
#7843=CARTESIAN_POINT('',(0.,0.,0.));
#7844=CARTESIAN_POINT('Origin',(6.5,-3.47,5.4));
#7845=CARTESIAN_POINT('',(6.19,-3.47,6.64));
#7846=CARTESIAN_POINT('Origin',(6.5,-3.47,6.64));
#7847=CARTESIAN_POINT('',(6.19,-3.47,5.4));
#7848=CARTESIAN_POINT('',(6.19,-3.47,5.4));
#7849=CARTESIAN_POINT('Origin',(6.5,-3.47,5.4));
#7850=CARTESIAN_POINT('Origin',(6.5,-3.47,5.4));
#7851=CARTESIAN_POINT('',(6.,-3.47,6.64));
#7852=CARTESIAN_POINT('Origin',(6.5,-3.47,6.64));
#7853=CARTESIAN_POINT('',(6.,-3.47,5.4));
#7854=CARTESIAN_POINT('',(6.,-3.47,5.4));
#7855=CARTESIAN_POINT('Origin',(6.5,-3.47,5.4));
#7856=CARTESIAN_POINT('Origin',(6.5,-3.47,6.64));
#7857=CARTESIAN_POINT('Origin',(6.5,-3.47,5.4));
#7858=CARTESIAN_POINT('',(0.,0.,0.));
#7859=CARTESIAN_POINT('Origin',(6.5,-3.47,6.64));
#7860=CARTESIAN_POINT('',(6.275,-3.47,6.84));
#7861=CARTESIAN_POINT('Origin',(6.5,-3.47,6.84));
#7862=CARTESIAN_POINT('',(6.275,-3.47,6.64));
#7863=CARTESIAN_POINT('',(6.275,-3.47,6.64));
#7864=CARTESIAN_POINT('Origin',(6.5,-3.47,6.64));
#7865=CARTESIAN_POINT('Origin',(6.5,-3.47,6.64));
#7866=CARTESIAN_POINT('',(5.8,-3.47,6.84));
#7867=CARTESIAN_POINT('Origin',(6.5,-3.47,6.84));
#7868=CARTESIAN_POINT('',(5.8,-3.47,6.64));
#7869=CARTESIAN_POINT('',(5.8,-3.47,6.64));
#7870=CARTESIAN_POINT('Origin',(6.5,-3.47,6.64));
#7871=CARTESIAN_POINT('Origin',(6.5,-3.47,6.84));
#7872=CARTESIAN_POINT('Origin',(6.5,-3.47,6.64));
#7873=CARTESIAN_POINT('',(0.,0.,0.));
#7874=CARTESIAN_POINT('Origin',(8.8,-2.47,0.9));
#7875=CARTESIAN_POINT('',(8.635,-2.47,1.));
#7876=CARTESIAN_POINT('Origin',(8.8,-2.47,1.));
#7877=CARTESIAN_POINT('',(8.635,-2.47,2.1));
#7878=CARTESIAN_POINT('',(8.635,-2.47,0.9));
#7879=CARTESIAN_POINT('Origin',(8.8,-2.47,2.1));
#7880=CARTESIAN_POINT('Origin',(8.8,-2.47,2.1));
#7881=CARTESIAN_POINT('Origin',(8.1,-2.69,6.1));
#7882=CARTESIAN_POINT('',(8.,-2.69,6.7));
#7883=CARTESIAN_POINT('Origin',(8.1,-2.69,6.7));
#7884=CARTESIAN_POINT('',(8.,-2.69,6.1));
#7885=CARTESIAN_POINT('',(8.,-2.69,6.1));
#7886=CARTESIAN_POINT('',(8.1,-2.79,6.1));
#7887=CARTESIAN_POINT('Origin',(8.1,-2.69,6.1));
#7888=CARTESIAN_POINT('Origin',(8.1,-2.69,6.1));
#7889=CARTESIAN_POINT('Origin',(8.1,-2.69,6.7));
#7890=CARTESIAN_POINT('Origin',(8.5,-2.43,6.1));
#7891=CARTESIAN_POINT('',(7.9,-2.07,6.1));
#7892=CARTESIAN_POINT('',(7.9,-2.79,6.1));
#7893=CARTESIAN_POINT('',(7.9,-2.07,6.1));
#7894=CARTESIAN_POINT('',(7.9,-2.79,6.1));
#7895=CARTESIAN_POINT('',(9.1,-2.79,6.1));
#7896=CARTESIAN_POINT('',(7.9,-2.79,6.1));
#7897=CARTESIAN_POINT('',(9.1,-2.07,6.1));
#7898=CARTESIAN_POINT('',(9.1,-2.79,6.1));
#7899=CARTESIAN_POINT('',(9.1,-2.07,6.1));
#7900=CARTESIAN_POINT('Origin',(8.5,-2.43,6.));
#7901=CARTESIAN_POINT('',(7.9,-2.07,6.));
#7902=CARTESIAN_POINT('',(7.9,-2.79,6.));
#7903=CARTESIAN_POINT('',(7.9,-2.07,6.));
#7904=CARTESIAN_POINT('',(9.1,-2.07,6.));
#7905=CARTESIAN_POINT('',(9.1,-2.07,6.));
#7906=CARTESIAN_POINT('',(9.1,-2.47,6.));
#7907=CARTESIAN_POINT('',(9.1,-2.79,6.));
#7908=CARTESIAN_POINT('',(8.5,-2.47,6.));
#7909=CARTESIAN_POINT('Origin',(8.8,-2.47,6.));
#7910=CARTESIAN_POINT('Origin',(8.8,-2.47,6.));
#7911=CARTESIAN_POINT('',(9.1,-2.79,6.));
#7912=CARTESIAN_POINT('',(9.1,-2.79,6.));
#7913=CARTESIAN_POINT('',(7.9,-2.79,6.));
#7914=CARTESIAN_POINT('Origin',(9.1,-2.07,6.));
#7915=CARTESIAN_POINT('',(7.9,-2.07,6.));
#7916=CARTESIAN_POINT('',(9.1,-2.07,6.));
#7917=CARTESIAN_POINT('Origin',(9.1,-2.79,6.));
#7918=CARTESIAN_POINT('',(9.1,-2.79,6.));
#7919=CARTESIAN_POINT('Origin',(7.9,-2.79,6.));
#7920=CARTESIAN_POINT('',(7.9,-2.79,6.));
#7921=CARTESIAN_POINT('Origin',(7.9,-2.07,6.));
#7922=CARTESIAN_POINT('Origin',(8.8,-2.47,1.));
#7923=CARTESIAN_POINT('',(8.5,-2.47,1.));
#7924=CARTESIAN_POINT('',(8.5,-2.47,1.));
#7925=CARTESIAN_POINT('Origin',(8.8,-2.47,1.));
#7926=CARTESIAN_POINT('Origin',(8.8,-2.47,1.));
#7927=CARTESIAN_POINT('',(0.,0.,0.));
#7928=CARTESIAN_POINT('Origin',(0.9,0.,1.4));
#7929=CARTESIAN_POINT('',(0.988888264668966,0.25,1.4));
#7930=CARTESIAN_POINT('',(1.02,-1.18386380373883E-17,1.65));
#7931=CARTESIAN_POINT('Ctrl Pts',(0.988888264668966,0.25,1.4));
#7932=CARTESIAN_POINT('Ctrl Pts',(0.988888264668966,0.25,1.43153139415882));
#7933=CARTESIAN_POINT('Ctrl Pts',(0.990553370646674,0.243672048431404,1.46507214966317));
#7934=CARTESIAN_POINT('Ctrl Pts',(0.996491737296663,0.218119830014375,1.52662620974954));
#7935=CARTESIAN_POINT('Ctrl Pts',(1.00067109353237,0.198902128206072,1.5546512623872));
#7936=CARTESIAN_POINT('Ctrl Pts',(1.00845756932386,0.154654113568716,1.59889927702456));
#7937=CARTESIAN_POINT('Ctrl Pts',(1.01258144235289,0.126627870945253,1.61811920309393));
#7938=CARTESIAN_POINT('Ctrl Pts',(1.0183917429657,0.065069600391363,1.64367304400768));
#7939=CARTESIAN_POINT('Ctrl Pts',(1.02,0.031527330883376,1.65));
#7940=CARTESIAN_POINT('Ctrl Pts',(1.02,2.77555756156289E-17,1.65));
#7941=CARTESIAN_POINT('Ctrl Pts',(1.02,6.93889390390723E-18,1.65));
#7942=CARTESIAN_POINT('Ctrl Pts',(1.02,-0.031527330883376,1.65));
#7943=CARTESIAN_POINT('Ctrl Pts',(1.0183917429657,-0.065069600391363,1.64367304400768));
#7944=CARTESIAN_POINT('Ctrl Pts',(1.01258144235289,-0.126627870945253,1.61811920309393));
#7945=CARTESIAN_POINT('Ctrl Pts',(1.00845756932386,-0.154654113568716,1.59889927702456));
#7946=CARTESIAN_POINT('Ctrl Pts',(1.00067109353237,-0.198902128206072,1.5546512623872));
#7947=CARTESIAN_POINT('Ctrl Pts',(0.996491737296663,-0.218119830014375,
1.52662620974954));
#7948=CARTESIAN_POINT('Ctrl Pts',(0.990553370646674,-0.243672048431404,
1.46507214966317));
#7949=CARTESIAN_POINT('Ctrl Pts',(0.988888264668967,-0.25,1.43153139415882));
#7950=CARTESIAN_POINT('Ctrl Pts',(0.988888264668967,-0.25,1.36846860584118));
#7951=CARTESIAN_POINT('Ctrl Pts',(0.990553370646674,-0.243672048431404,
1.33492785033683));
#7952=CARTESIAN_POINT('Ctrl Pts',(0.996491737296663,-0.218119830014375,
1.27337379025046));
#7953=CARTESIAN_POINT('Ctrl Pts',(1.00067109353237,-0.198902128206072,1.2453487376128));
#7954=CARTESIAN_POINT('Ctrl Pts',(1.00845756932386,-0.154654113568716,1.20110072297544));
#7955=CARTESIAN_POINT('Ctrl Pts',(1.01258144235289,-0.126627870945254,1.18188079690607));
#7956=CARTESIAN_POINT('Ctrl Pts',(1.0183917429657,-0.0650696003913633,1.15632695599232));
#7957=CARTESIAN_POINT('Ctrl Pts',(1.02,-0.0315273308833761,1.15));
#7958=CARTESIAN_POINT('Ctrl Pts',(1.02,0.0315273308833759,1.15));
#7959=CARTESIAN_POINT('Ctrl Pts',(1.0183917429657,0.065069600391363,1.15632695599232));
#7960=CARTESIAN_POINT('Ctrl Pts',(1.01258144235289,0.126627870945253,1.18188079690607));
#7961=CARTESIAN_POINT('Ctrl Pts',(1.00845756932386,0.154654113568716,1.20110072297544));
#7962=CARTESIAN_POINT('Ctrl Pts',(1.00067109353237,0.198902128206072,1.2453487376128));
#7963=CARTESIAN_POINT('Ctrl Pts',(0.996491737296663,0.218119830014375,1.27337379025046));
#7964=CARTESIAN_POINT('Ctrl Pts',(0.990553370646674,0.243672048431404,1.33492785033683));
#7965=CARTESIAN_POINT('Ctrl Pts',(0.988888264668967,0.25,1.36846860584118));
#7966=CARTESIAN_POINT('Ctrl Pts',(0.988888264668967,0.25,1.4));
#7967=CARTESIAN_POINT('',(3.,-3.06161699786838E-17,1.65));
#7968=CARTESIAN_POINT('',(0.9,-3.06161699786838E-17,1.65));
#7969=CARTESIAN_POINT('',(2.98956518577535,0.25,1.4));
#7970=CARTESIAN_POINT('Ctrl Pts',(2.98956518577535,0.25,1.4));
#7971=CARTESIAN_POINT('Ctrl Pts',(2.98956518577535,0.25,1.36859378633186));
#7972=CARTESIAN_POINT('Ctrl Pts',(2.99011104995181,0.24372047740942,1.33510417960069));
#7973=CARTESIAN_POINT('Ctrl Pts',(2.99208145165098,0.218202539734559,1.27351367328886));
#7974=CARTESIAN_POINT('Ctrl Pts',(2.99347740802958,0.198964922639276,1.245411532046));
#7975=CARTESIAN_POINT('Ctrl Pts',(2.99609686518216,0.154588504271054,1.20103511367778));
#7976=CARTESIAN_POINT('Ctrl Pts',(2.99749070376198,0.126486346986081,1.18179746841036));
#7977=CARTESIAN_POINT('Ctrl Pts',(2.99945625936844,0.0648957875009219,1.15627950921557));
#7978=CARTESIAN_POINT('Ctrl Pts',(3.,0.0314061622633416,1.15));
#7979=CARTESIAN_POINT('Ctrl Pts',(3.,-0.0314061622633416,1.15));
#7980=CARTESIAN_POINT('Ctrl Pts',(2.99945625936844,-0.0648957875009221,
1.15627950921557));
#7981=CARTESIAN_POINT('Ctrl Pts',(2.99749070376198,-0.126486346986081,1.18179746841036));
#7982=CARTESIAN_POINT('Ctrl Pts',(2.99609686518216,-0.154588504271054,1.20103511367778));
#7983=CARTESIAN_POINT('Ctrl Pts',(2.99347740802958,-0.198964922639276,1.245411532046));
#7984=CARTESIAN_POINT('Ctrl Pts',(2.99208145165098,-0.218202539734559,1.27351367328886));
#7985=CARTESIAN_POINT('Ctrl Pts',(2.99011104995181,-0.24372047740942,1.33510417960069));
#7986=CARTESIAN_POINT('Ctrl Pts',(2.98956518577535,-0.25,1.36859378633186));
#7987=CARTESIAN_POINT('Ctrl Pts',(2.98956518577535,-0.25,1.43140621366814));
#7988=CARTESIAN_POINT('Ctrl Pts',(2.99011104995181,-0.24372047740942,1.4648958203993));
#7989=CARTESIAN_POINT('Ctrl Pts',(2.99208145165098,-0.21820253973456,1.52648632671114));
#7990=CARTESIAN_POINT('Ctrl Pts',(2.99347740802958,-0.198964922639276,1.554588467954));
#7991=CARTESIAN_POINT('Ctrl Pts',(2.99609686518216,-0.154588504271054,1.59896488632222));
#7992=CARTESIAN_POINT('Ctrl Pts',(2.99749070376198,-0.126486346986082,1.61820253158964));
#7993=CARTESIAN_POINT('Ctrl Pts',(2.99945625936844,-0.0648957875009221,
1.64372049078443));
#7994=CARTESIAN_POINT('Ctrl Pts',(3.,-0.0314061622633417,1.65));
#7995=CARTESIAN_POINT('Ctrl Pts',(3.,-5.55111512312578E-17,1.65));
#7996=CARTESIAN_POINT('Ctrl Pts',(3.,-2.08166817117217E-17,1.65));
#7997=CARTESIAN_POINT('Ctrl Pts',(3.,0.0314061622633416,1.65));
#7998=CARTESIAN_POINT('Ctrl Pts',(2.99945625936844,0.0648957875009221,1.64372049078443));
#7999=CARTESIAN_POINT('Ctrl Pts',(2.99749070376198,0.126486346986081,1.61820253158964));
#8000=CARTESIAN_POINT('Ctrl Pts',(2.99609686518216,0.154588504271054,1.59896488632222));
#8001=CARTESIAN_POINT('Ctrl Pts',(2.99347740802958,0.198964922639276,1.554588467954));
#8002=CARTESIAN_POINT('Ctrl Pts',(2.99208145165098,0.218202539734559,1.52648632671114));
#8003=CARTESIAN_POINT('Ctrl Pts',(2.99011104995181,0.24372047740942,1.46489582039931));
#8004=CARTESIAN_POINT('Ctrl Pts',(2.98956518577535,0.25,1.43140621366814));
#8005=CARTESIAN_POINT('Ctrl Pts',(2.98956518577535,0.25,1.4));
#8006=CARTESIAN_POINT('Origin',(-1.23743686707646,-1.23743686707646,2.9));
#8007=CARTESIAN_POINT('',(-1.40243686707646,-1.23743686707646,2.9));
#8008=CARTESIAN_POINT('Origin',(-1.23743686707646,-1.23743686707646,2.9));
#8009=CARTESIAN_POINT('',(-1.40243686707646,-1.23743686707646,3.6));
#8010=CARTESIAN_POINT('',(-1.40243686707646,-1.23743686707646,2.9));
#8011=CARTESIAN_POINT('Origin',(-1.23743686707646,-1.23743686707646,3.6));
#8012=CARTESIAN_POINT('Origin',(-1.23743686707646,-1.23743686707646,2.9));
#8013=CARTESIAN_POINT('Origin',(-1.23743686707646,1.23743686707646,2.9));
#8014=CARTESIAN_POINT('',(-1.40243686707646,1.23743686707646,2.9));
#8015=CARTESIAN_POINT('Origin',(-1.23743686707646,1.23743686707646,2.9));
#8016=CARTESIAN_POINT('',(-1.40243686707646,1.23743686707646,3.6));
#8017=CARTESIAN_POINT('',(-1.40243686707646,1.23743686707646,2.9));
#8018=CARTESIAN_POINT('Origin',(-1.23743686707646,1.23743686707646,3.6));
#8019=CARTESIAN_POINT('Origin',(-1.23743686707646,1.23743686707646,2.9));
#8020=CARTESIAN_POINT('Origin',(1.23743686707646,1.23743686707646,2.9));
#8021=CARTESIAN_POINT('',(1.07243686707646,1.23743686707646,2.9));
#8022=CARTESIAN_POINT('Origin',(1.23743686707646,1.23743686707646,2.9));
#8023=CARTESIAN_POINT('',(1.07243686707646,1.23743686707646,3.6));
#8024=CARTESIAN_POINT('',(1.07243686707646,1.23743686707646,2.9));
#8025=CARTESIAN_POINT('Origin',(1.23743686707646,1.23743686707646,3.6));
#8026=CARTESIAN_POINT('Origin',(1.23743686707646,1.23743686707646,2.9));
#8027=CARTESIAN_POINT('Origin',(1.23743686707646,-1.23743686707646,2.9));
#8028=CARTESIAN_POINT('',(1.07243686707646,-1.23743686707646,2.9));
#8029=CARTESIAN_POINT('Origin',(1.23743686707646,-1.23743686707646,2.9));
#8030=CARTESIAN_POINT('',(1.07243686707646,-1.23743686707646,3.6));
#8031=CARTESIAN_POINT('',(1.07243686707646,-1.23743686707646,2.9));
#8032=CARTESIAN_POINT('Origin',(1.23743686707646,-1.23743686707646,3.6));
#8033=CARTESIAN_POINT('Origin',(1.23743686707646,-1.23743686707646,2.9));
#8034=CARTESIAN_POINT('Origin',(-1.76776695296637,-1.76776695296637,2.4));
#8035=CARTESIAN_POINT('',(-1.8139637388702,-1.24480341984751,2.4));
#8036=CARTESIAN_POINT('',(-1.24480341984751,-1.81396373887019,2.4));
#8037=CARTESIAN_POINT('Origin',(0.,0.,2.4));
#8038=CARTESIAN_POINT('Origin',(-1.76776695296637,-1.76776695296637,2.4));
#8039=CARTESIAN_POINT('Origin',(-1.76776695296637,-1.76776695296637,1.8));
#8040=CARTESIAN_POINT('',(-1.8139637388702,-1.24480341984751,1.8));
#8041=CARTESIAN_POINT('',(-1.8139637388702,-1.24480341984751,1.8));
#8042=CARTESIAN_POINT('',(-1.24480341984751,-1.81396373887019,1.8));
#8043=CARTESIAN_POINT('Origin',(-1.76776695296637,-1.76776695296637,1.8));
#8044=CARTESIAN_POINT('',(-1.24480341984751,-1.81396373887019,1.8));
#8045=CARTESIAN_POINT('Origin',(-1.76776695296637,1.76776695296637,1.8));
#8046=CARTESIAN_POINT('',(-1.81396373887019,1.24480341984751,2.4));
#8047=CARTESIAN_POINT('',(-1.81396373887019,1.24480341984751,1.8));
#8048=CARTESIAN_POINT('',(-1.81396373887019,1.24480341984751,1.8));
#8049=CARTESIAN_POINT('',(-1.24480341984751,1.81396373887019,2.4));
#8050=CARTESIAN_POINT('Origin',(-1.76776695296637,1.76776695296637,2.4));
#8051=CARTESIAN_POINT('',(-1.24480341984751,1.81396373887019,1.8));
#8052=CARTESIAN_POINT('',(-1.24480341984751,1.81396373887019,1.8));
#8053=CARTESIAN_POINT('Origin',(-1.76776695296637,1.76776695296637,1.8));
#8054=CARTESIAN_POINT('Origin',(-1.76776695296637,1.76776695296637,2.4));
#8055=CARTESIAN_POINT('Origin',(0.,0.,2.4));
#8056=CARTESIAN_POINT('Origin',(1.76776695296637,1.76776695296637,1.8));
#8057=CARTESIAN_POINT('',(1.24480341984751,1.81396373887019,2.4));
#8058=CARTESIAN_POINT('',(1.24480341984751,1.81396373887019,1.8));
#8059=CARTESIAN_POINT('',(1.24480341984751,1.81396373887019,1.8));
#8060=CARTESIAN_POINT('',(1.81396373887019,1.24480341984751,2.4));
#8061=CARTESIAN_POINT('Origin',(1.76776695296637,1.76776695296637,2.4));
#8062=CARTESIAN_POINT('',(1.81396373887019,1.24480341984751,1.8));
#8063=CARTESIAN_POINT('',(1.81396373887019,1.24480341984751,1.8));
#8064=CARTESIAN_POINT('Origin',(1.76776695296637,1.76776695296637,1.8));
#8065=CARTESIAN_POINT('Origin',(1.76776695296637,1.76776695296637,2.4));
#8066=CARTESIAN_POINT('Origin',(0.,0.,2.4));
#8067=CARTESIAN_POINT('Origin',(1.76776695296637,-1.76776695296637,1.8));
#8068=CARTESIAN_POINT('',(1.81396373887019,-1.24480341984751,2.4));
#8069=CARTESIAN_POINT('',(1.81396373887019,-1.24480341984751,1.8));
#8070=CARTESIAN_POINT('',(1.81396373887019,-1.24480341984751,1.8));
#8071=CARTESIAN_POINT('',(1.24480341984751,-1.8139637388702,2.4));
#8072=CARTESIAN_POINT('Origin',(1.76776695296637,-1.76776695296637,2.4));
#8073=CARTESIAN_POINT('',(1.24480341984751,-1.8139637388702,1.8));
#8074=CARTESIAN_POINT('',(1.24480341984751,-1.8139637388702,1.8));
#8075=CARTESIAN_POINT('Origin',(1.76776695296637,-1.76776695296637,1.8));
#8076=CARTESIAN_POINT('Origin',(1.76776695296637,-1.76776695296637,2.4));
#8077=CARTESIAN_POINT('Origin',(0.,0.,2.4));
#8078=CARTESIAN_POINT('Origin',(0.,0.,1.));
#8079=CARTESIAN_POINT('',(-2.2,-2.69422295812418E-16,3.6));
#8080=CARTESIAN_POINT('Origin',(0.,0.,3.6));
#8081=CARTESIAN_POINT('',(-2.2,-2.69422295812418E-16,1.8));
#8082=CARTESIAN_POINT('',(-2.2,-2.69422295812418E-16,1.));
#8083=CARTESIAN_POINT('Origin',(0.,0.,1.8));
#8084=CARTESIAN_POINT('Origin',(0.,0.,1.8));
#8085=CARTESIAN_POINT('Origin',(0.,0.,1.8));
#8086=CARTESIAN_POINT('Origin',(0.,0.,1.8));
#8087=CARTESIAN_POINT('Origin',(0.,0.,1.8));
#8088=CARTESIAN_POINT('Origin',(0.,0.,1.8));
#8089=CARTESIAN_POINT('',(-3.,-3.67394039744206E-16,1.8));
#8090=CARTESIAN_POINT('Origin',(0.,0.,1.8));
#8091=CARTESIAN_POINT('',(-2.04276695296637,-1.76776695296637,1.8));
#8092=CARTESIAN_POINT('Origin',(-1.76776695296637,-1.76776695296637,1.8));
#8093=CARTESIAN_POINT('',(1.49276695296637,1.76776695296637,1.8));
#8094=CARTESIAN_POINT('Origin',(1.76776695296637,1.76776695296637,1.8));
#8095=CARTESIAN_POINT('',(1.49276695296637,-1.76776695296637,1.8));
#8096=CARTESIAN_POINT('Origin',(1.76776695296637,-1.76776695296637,1.8));
#8097=CARTESIAN_POINT('',(-2.04276695296637,1.76776695296637,1.8));
#8098=CARTESIAN_POINT('Origin',(-1.76776695296637,1.76776695296637,1.8));
#8099=CARTESIAN_POINT('Origin',(-1.76776695296637,-1.76776695296637,0.9));
#8100=CARTESIAN_POINT('',(-2.04276695296637,-1.76776695296637,1.));
#8101=CARTESIAN_POINT('Origin',(-1.76776695296637,-1.76776695296637,1.));
#8102=CARTESIAN_POINT('',(-2.04276695296637,-1.76776695296637,0.9));
#8103=CARTESIAN_POINT('Origin',(-1.76776695296637,1.76776695296637,0.9));
#8104=CARTESIAN_POINT('',(-2.04276695296637,1.76776695296637,1.));
#8105=CARTESIAN_POINT('Origin',(-1.76776695296637,1.76776695296637,1.));
#8106=CARTESIAN_POINT('',(-2.04276695296637,1.76776695296637,0.9));
#8107=CARTESIAN_POINT('Origin',(1.76776695296637,1.76776695296637,0.9));
#8108=CARTESIAN_POINT('',(1.49276695296637,1.76776695296637,1.));
#8109=CARTESIAN_POINT('Origin',(1.76776695296637,1.76776695296637,1.));
#8110=CARTESIAN_POINT('',(1.49276695296637,1.76776695296637,0.9));
#8111=CARTESIAN_POINT('Origin',(1.76776695296637,-1.76776695296637,0.9));
#8112=CARTESIAN_POINT('',(1.49276695296637,-1.76776695296637,1.));
#8113=CARTESIAN_POINT('Origin',(1.76776695296637,-1.76776695296637,1.));
#8114=CARTESIAN_POINT('',(1.49276695296637,-1.76776695296637,0.9));
#8115=CARTESIAN_POINT('Origin',(0.,0.,2.05));
#8116=CARTESIAN_POINT('',(-1.5,-1.83697019872103E-16,2.05));
#8117=CARTESIAN_POINT('Origin',(0.,0.,2.05));
#8118=CARTESIAN_POINT('',(-1.5,1.83697019872103E-16,3.6));
#8119=CARTESIAN_POINT('',(-1.5,-1.83697019872103E-16,2.05));
#8120=CARTESIAN_POINT('Origin',(0.,0.,3.6));
#8121=CARTESIAN_POINT('Origin',(0.,0.,2.05));
#8122=CARTESIAN_POINT('',(-1.02,-1.2491397351303E-16,2.05));
#8123=CARTESIAN_POINT('Origin',(0.,0.,2.05));
#8124=CARTESIAN_POINT('Origin',(0.,0.,1.));
#8125=CARTESIAN_POINT('',(-3.,-3.67394039744206E-16,1.));
#8126=CARTESIAN_POINT('',(-3.,-3.67394039744206E-16,1.));
#8127=CARTESIAN_POINT('Origin',(0.,0.,1.));
#8128=CARTESIAN_POINT('Origin',(0.,0.,1.));
#8129=CARTESIAN_POINT('',(-1.02,-1.2491397351303E-16,1.));
#8130=CARTESIAN_POINT('',(-1.02,-1.2491397351303E-16,1.));
#8131=CARTESIAN_POINT('Origin',(0.,0.,1.));
#8132=CARTESIAN_POINT('Origin',(0.,0.,3.6));
#8133=CARTESIAN_POINT('Origin',(0.,0.,1.));
#8134=CARTESIAN_POINT('',(0.,0.,0.));
#8135=CARTESIAN_POINT('Origin',(-1.23743686707646,-1.23743686707646,4.));
#8136=CARTESIAN_POINT('',(-1.61243686707646,-1.23743686707646,4.));
#8137=CARTESIAN_POINT('Origin',(-1.23743686707646,-1.23743686707646,4.));
#8138=CARTESIAN_POINT('',(-1.61243686707646,-1.23743686707646,4.4));
#8139=CARTESIAN_POINT('',(-1.61243686707646,-1.23743686707646,4.));
#8140=CARTESIAN_POINT('Origin',(-1.23743686707646,-1.23743686707646,4.4));
#8141=CARTESIAN_POINT('Origin',(-1.23743686707646,-1.23743686707646,4.));
#8142=CARTESIAN_POINT('',(-1.46243686707646,-1.23743686707646,4.));
#8143=CARTESIAN_POINT('Origin',(-1.23743686707646,-1.23743686707646,4.));
#8144=CARTESIAN_POINT('Origin',(-1.23743686707646,1.23743686707646,4.));
#8145=CARTESIAN_POINT('',(-1.61243686707646,1.23743686707646,4.));
#8146=CARTESIAN_POINT('Origin',(-1.23743686707646,1.23743686707646,4.));
#8147=CARTESIAN_POINT('',(-1.61243686707646,1.23743686707646,4.4));
#8148=CARTESIAN_POINT('',(-1.61243686707646,1.23743686707646,4.));
#8149=CARTESIAN_POINT('Origin',(-1.23743686707646,1.23743686707646,4.4));
#8150=CARTESIAN_POINT('Origin',(-1.23743686707646,1.23743686707646,4.));
#8151=CARTESIAN_POINT('',(-1.46243686707646,1.23743686707646,4.));
#8152=CARTESIAN_POINT('Origin',(-1.23743686707646,1.23743686707646,4.));
#8153=CARTESIAN_POINT('Origin',(1.23743686707646,1.23743686707646,4.));
#8154=CARTESIAN_POINT('',(0.862436867076458,1.23743686707646,4.));
#8155=CARTESIAN_POINT('Origin',(1.23743686707646,1.23743686707646,4.));
#8156=CARTESIAN_POINT('',(0.862436867076458,1.23743686707646,4.4));
#8157=CARTESIAN_POINT('',(0.862436867076458,1.23743686707646,4.));
#8158=CARTESIAN_POINT('Origin',(1.23743686707646,1.23743686707646,4.4));
#8159=CARTESIAN_POINT('Origin',(1.23743686707646,1.23743686707646,4.));
#8160=CARTESIAN_POINT('',(1.01243686707646,1.23743686707646,4.));
#8161=CARTESIAN_POINT('Origin',(1.23743686707646,1.23743686707646,4.));
#8162=CARTESIAN_POINT('Origin',(1.23743686707646,-1.23743686707646,4.));
#8163=CARTESIAN_POINT('',(0.862436867076458,-1.23743686707646,4.));
#8164=CARTESIAN_POINT('Origin',(1.23743686707646,-1.23743686707646,4.));
#8165=CARTESIAN_POINT('',(0.862436867076458,-1.23743686707646,4.4));
#8166=CARTESIAN_POINT('',(0.862436867076458,-1.23743686707646,4.));
#8167=CARTESIAN_POINT('Origin',(1.23743686707646,-1.23743686707646,4.4));
#8168=CARTESIAN_POINT('Origin',(1.23743686707646,-1.23743686707646,4.));
#8169=CARTESIAN_POINT('',(1.01243686707646,-1.23743686707646,4.));
#8170=CARTESIAN_POINT('Origin',(1.23743686707646,-1.23743686707646,4.));
#8171=CARTESIAN_POINT('Origin',(-1.23743686707646,-1.23743686707646,3.5));
#8172=CARTESIAN_POINT('',(-1.46243686707646,-1.23743686707646,3.6));
#8173=CARTESIAN_POINT('Origin',(-1.23743686707646,-1.23743686707646,3.6));
#8174=CARTESIAN_POINT('',(-1.46243686707646,-1.23743686707646,3.5));
#8175=CARTESIAN_POINT('Origin',(-1.23743686707646,1.23743686707646,3.5));
#8176=CARTESIAN_POINT('',(-1.46243686707646,1.23743686707646,3.6));
#8177=CARTESIAN_POINT('Origin',(-1.23743686707646,1.23743686707646,3.6));
#8178=CARTESIAN_POINT('',(-1.46243686707646,1.23743686707646,3.5));
#8179=CARTESIAN_POINT('Origin',(1.23743686707646,1.23743686707646,3.5));
#8180=CARTESIAN_POINT('',(1.01243686707646,1.23743686707646,3.6));
#8181=CARTESIAN_POINT('Origin',(1.23743686707646,1.23743686707646,3.6));
#8182=CARTESIAN_POINT('',(1.01243686707646,1.23743686707646,3.5));
#8183=CARTESIAN_POINT('Origin',(1.23743686707646,-1.23743686707646,3.5));
#8184=CARTESIAN_POINT('',(1.01243686707646,-1.23743686707646,3.6));
#8185=CARTESIAN_POINT('Origin',(1.23743686707646,-1.23743686707646,3.6));
#8186=CARTESIAN_POINT('',(1.01243686707646,-1.23743686707646,3.5));
#8187=CARTESIAN_POINT('Origin',(0.,0.,2.95));
#8188=CARTESIAN_POINT('',(-1.49,-1.82472373072956E-16,3.6));
#8189=CARTESIAN_POINT('Origin',(0.,0.,3.6));
#8190=CARTESIAN_POINT('',(-1.49,-1.82472373072956E-16,2.95));
#8191=CARTESIAN_POINT('',(-1.49,-1.82472373072956E-16,2.95));
#8192=CARTESIAN_POINT('Origin',(0.,0.,2.95));
#8193=CARTESIAN_POINT('Origin',(0.,0.,2.95));
#8194=CARTESIAN_POINT('',(-0.71,-8.69499227394621E-17,2.95));
#8195=CARTESIAN_POINT('Origin',(0.,0.,2.95));
#8196=CARTESIAN_POINT('Origin',(0.,0.,3.6));
#8197=CARTESIAN_POINT('',(-0.71,-8.69499227394621E-17,4.4));
#8198=CARTESIAN_POINT('Origin',(0.,0.,4.4));
#8199=CARTESIAN_POINT('',(-0.71,-8.69499227394621E-17,3.6));
#8200=CARTESIAN_POINT('Origin',(0.,0.,3.6));
#8201=CARTESIAN_POINT('',(-2.2,-2.69422295812418E-16,4.4));
#8202=CARTESIAN_POINT('Origin',(0.,0.,4.4));
#8203=CARTESIAN_POINT('',(-2.2,-2.69422295812418E-16,3.6));
#8204=CARTESIAN_POINT('',(-2.2,-2.69422295812418E-16,3.6));
#8205=CARTESIAN_POINT('Origin',(0.,0.,3.6));
#8206=CARTESIAN_POINT('Origin',(0.,0.,4.4));
#8207=CARTESIAN_POINT('Origin',(0.,0.,3.6));
#8208=CARTESIAN_POINT('',(0.,0.,0.));
#8209=CARTESIAN_POINT('',(0.,0.,0.));
#8210=CARTESIAN_POINT('Origin',(0.,0.,0.));
#8211=CARTESIAN_POINT('',(-0.976185,-0.246528389340863,-1.19548183562566E-16));
#8212=CARTESIAN_POINT('',(-1.19548183562566E-16,-0.246528389340863,0.976185));
#8213=CARTESIAN_POINT('Origin',(0.,-0.246528389340863,0.));
#8214=CARTESIAN_POINT('Origin',(0.,-0.246528389340863,0.));
#8215=CARTESIAN_POINT('',(-1.19548183562566E-16,0.246528389340863,0.976185));
#8216=CARTESIAN_POINT('Origin',(-1.22464679914735E-16,0.,1.));
#8217=CARTESIAN_POINT('',(-0.976185,0.246528389340863,1.19548183562566E-16));
#8218=CARTESIAN_POINT('Origin',(0.,0.246528389340863,0.));
#8219=CARTESIAN_POINT('Origin',(0.,0.246528389340863,0.));
#8220=CARTESIAN_POINT('Origin',(0.,0.,0.));
#8221=CARTESIAN_POINT('',(-0.976185,0.45,-1.19548183562566E-16));
#8222=CARTESIAN_POINT('',(-0.976185,0.,-1.19548183562566E-16));
#8223=CARTESIAN_POINT('Origin',(0.,0.45,0.));
#8224=CARTESIAN_POINT('Origin',(0.,0.,0.));
#8225=CARTESIAN_POINT('',(-0.5,-0.39,-6.12323399573677E-17));
#8226=CARTESIAN_POINT('Origin',(0.,-0.39,0.));
#8227=CARTESIAN_POINT('',(-0.5,0.39,-6.12323399573677E-17));
#8228=CARTESIAN_POINT('',(-0.5,0.,-6.12323399573677E-17));
#8229=CARTESIAN_POINT('Origin',(0.,0.39,0.));
#8230=CARTESIAN_POINT('Origin',(0.,0.42,0.));
#8231=CARTESIAN_POINT('',(-0.56,0.45,-6.85802207522518E-17));
#8232=CARTESIAN_POINT('',(-0.53,0.42,-6.49062803548097E-17));
#8233=CARTESIAN_POINT('Origin',(0.,0.45,0.));
#8234=CARTESIAN_POINT('Origin',(0.976185,0.45,0.));
#8235=CARTESIAN_POINT('Origin',(0.,0.,0.));
#8236=CARTESIAN_POINT('',(-0.976185,-0.45,-1.19548183562566E-16));
#8237=CARTESIAN_POINT('Origin',(0.,-0.45,0.));
#8238=CARTESIAN_POINT('',(-0.976185,0.,-1.19548183562566E-16));
#8239=CARTESIAN_POINT('Origin',(0.56,-0.45,0.));
#8240=CARTESIAN_POINT('',(-0.56,-0.45,-6.85802207522518E-17));
#8241=CARTESIAN_POINT('Origin',(0.,-0.45,0.));
#8242=CARTESIAN_POINT('Origin',(0.,-0.42,0.));
#8243=CARTESIAN_POINT('',(-0.53,-0.42,-6.49062803548097E-17));
#8244=CARTESIAN_POINT('',(0.,0.,0.));
#8245=CARTESIAN_POINT('Origin',(0.,0.,0.));
#8246=CARTESIAN_POINT('',(-1.023815,0.246528389340863,-1.25381176266905E-16));
#8247=CARTESIAN_POINT('',(-1.25381176266905E-16,0.246528389340863,1.023815));
#8248=CARTESIAN_POINT('Origin',(0.,0.246528389340863,0.));
#8249=CARTESIAN_POINT('Origin',(0.,0.246528389340863,0.));
#8250=CARTESIAN_POINT('',(-1.25381176266905E-16,-0.246528389340863,1.023815));
#8251=CARTESIAN_POINT('Origin',(-1.22464679914735E-16,0.,1.));
#8252=CARTESIAN_POINT('',(-1.023815,-0.246528389340863,1.25381176266905E-16));
#8253=CARTESIAN_POINT('Origin',(0.,-0.246528389340863,0.));
#8254=CARTESIAN_POINT('Origin',(0.,-0.246528389340863,0.));
#8255=CARTESIAN_POINT('Origin',(0.,0.,0.));
#8256=CARTESIAN_POINT('',(-1.023815,-0.45,-1.25381176266905E-16));
#8257=CARTESIAN_POINT('Origin',(0.,-0.45,0.));
#8258=CARTESIAN_POINT('',(-1.023815,0.,-1.25381176266905E-16));
#8259=CARTESIAN_POINT('Origin',(1.44,0.45,0.));
#8260=CARTESIAN_POINT('',(-1.44,0.45,-1.76349139077219E-16));
#8261=CARTESIAN_POINT('Origin',(0.,0.45,0.));
#8262=CARTESIAN_POINT('',(-1.023815,0.45,-1.25381176266905E-16));
#8263=CARTESIAN_POINT('Origin',(0.,0.45,0.));
#8264=CARTESIAN_POINT('Origin',(0.,0.42,0.));
#8265=CARTESIAN_POINT('',(-1.5,0.39,-1.83697019872103E-16));
#8266=CARTESIAN_POINT('Origin',(0.,0.39,0.));
#8267=CARTESIAN_POINT('',(-1.47,0.42,-1.80023079474661E-16));
#8268=CARTESIAN_POINT('Origin',(0.,0.,0.));
#8269=CARTESIAN_POINT('',(-1.5,-0.39,-1.83697019872103E-16));
#8270=CARTESIAN_POINT('Origin',(0.,-0.39,0.));
#8271=CARTESIAN_POINT('',(-1.5,0.,-1.83697019872103E-16));
#8272=CARTESIAN_POINT('Origin',(0.,-0.42,0.));
#8273=CARTESIAN_POINT('',(-1.44,-0.45,-1.76349139077219E-16));
#8274=CARTESIAN_POINT('Origin',(0.,-0.45,0.));
#8275=CARTESIAN_POINT('',(-1.47,-0.42,-1.80023079474661E-16));
#8276=CARTESIAN_POINT('Origin',(1.023815,-0.45,0.));
#8277=CARTESIAN_POINT('Origin',(0.,0.,0.));
#8278=CARTESIAN_POINT('',(-1.023815,0.,-1.25381176266905E-16));
#8279=CARTESIAN_POINT('',(0.,0.,0.));
#8280=CARTESIAN_POINT('Origin',(1.,0.,0.));
#8281=CARTESIAN_POINT('',(1.,-1.78583896120461E-33,0.23815));
#8282=CARTESIAN_POINT('',(1.,-1.78583896120461E-33,-0.23815));
#8283=CARTESIAN_POINT('Origin',(1.,0.,0.));
#8284=CARTESIAN_POINT('Origin',(0.707106781186548,0.,-0.707106781186547));
#8285=CARTESIAN_POINT('',(0.875504261126124,-1.78583896120461E-33,-0.538709301246971));
#8286=CARTESIAN_POINT('',(0.538709301246971,-1.78583896120461E-33,-0.875504261126124));
#8287=CARTESIAN_POINT('Origin',(0.707106781186548,0.,-0.707106781186547));
#8288=CARTESIAN_POINT('Origin',(6.12323399573677E-17,0.,-1.));
#8289=CARTESIAN_POINT('',(0.23815,-1.78583896120461E-33,-1.));
#8290=CARTESIAN_POINT('',(-0.23815,-1.78583896120461E-33,-1.));
#8291=CARTESIAN_POINT('Origin',(6.12323399573677E-17,0.,-1.));
#8292=CARTESIAN_POINT('Origin',(-0.707106781186547,0.,-0.707106781186548));
#8293=CARTESIAN_POINT('',(-0.538709301246971,-1.78583896120461E-33,-0.875504261126124));
#8294=CARTESIAN_POINT('',(-0.875504261126124,-1.78583896120461E-33,-0.538709301246971));
#8295=CARTESIAN_POINT('Origin',(-0.707106781186547,0.,-0.707106781186548));
#8296=CARTESIAN_POINT('Origin',(-1.,0.,-1.22464679914735E-16));
#8297=CARTESIAN_POINT('',(-1.,-1.78583896120461E-33,-0.23815));
#8298=CARTESIAN_POINT('',(-1.,-1.78583896120461E-33,0.23815));
#8299=CARTESIAN_POINT('Origin',(-1.,0.,-1.22464679914735E-16));
#8300=CARTESIAN_POINT('Origin',(-0.707106781186548,0.,0.707106781186547));
#8301=CARTESIAN_POINT('',(-0.875504261126124,-7.94881478324376E-33,0.538709301246971));
#8302=CARTESIAN_POINT('',(-0.538709301246971,4.37713686083455E-33,0.875504261126124));
#8303=CARTESIAN_POINT('Origin',(-0.707106781186548,0.,0.707106781186547));
#8304=CARTESIAN_POINT('Origin',(-1.83697019872103E-16,0.,1.));
#8305=CARTESIAN_POINT('',(-0.23815,-1.78583896120461E-33,1.));
#8306=CARTESIAN_POINT('',(0.23815,-1.78583896120461E-33,1.));
#8307=CARTESIAN_POINT('Origin',(-1.83697019872103E-16,0.,1.));
#8308=CARTESIAN_POINT('Origin',(0.707106781186547,0.,0.707106781186548));
#8309=CARTESIAN_POINT('',(0.538709301246971,-4.86732687222419E-33,0.875504261126124));
#8310=CARTESIAN_POINT('',(0.875504261126124,1.29564894981497E-33,0.538709301246971));
#8311=CARTESIAN_POINT('Origin',(0.707106781186547,0.,0.707106781186548));
#8312=CARTESIAN_POINT('',(0.,0.,0.));
#8313=CARTESIAN_POINT('Origin',(0.707106781186547,0.,0.707106781186548));
#8314=CARTESIAN_POINT('',(0.504455939115715,-0.04763,0.841298510752802));
#8315=CARTESIAN_POINT('',(0.841298510752802,-0.04763,0.504455939115715));
#8316=CARTESIAN_POINT('Ctrl Pts',(0.504455939115715,-0.04763,0.841298510752802));
#8317=CARTESIAN_POINT('Ctrl Pts',(0.508899795931835,-0.0740444353928835,
0.838633903678357));
#8318=CARTESIAN_POINT('Ctrl Pts',(0.517157748491652,-0.0999305678883309,
0.833661031856294));
#8319=CARTESIAN_POINT('Ctrl Pts',(0.537715343527944,-0.142345102874864,
0.820511285096538));
#8320=CARTESIAN_POINT('Ctrl Pts',(0.548874290046456,-0.159766064500479,
0.813159949759));
#8321=CARTESIAN_POINT('Ctrl Pts',(0.573915184558107,-0.190326085855194,
0.795684265985089));
#8322=CARTESIAN_POINT('Ctrl Pts',(0.587792702767295,-0.203463743702801,
0.78555112003688));
#8323=CARTESIAN_POINT('Ctrl Pts',(0.615966552324775,-0.224161999508995,
0.763642258217233));
#8324=CARTESIAN_POINT('Ctrl Pts',(0.631684198665438,-0.232861760990032,
0.750785745543687));
#8325=CARTESIAN_POINT('Ctrl Pts',(0.663382628119203,-0.244251601209411,
0.722929908501543));
#8326=CARTESIAN_POINT('Ctrl Pts',(0.679352081686668,-0.246942143572133,
0.707917883896095));
#8327=CARTESIAN_POINT('Ctrl Pts',(0.707917883896095,-0.246942143572133,
0.679352081686668));
#8328=CARTESIAN_POINT('Ctrl Pts',(0.722929908501543,-0.244251601209411,
0.663382628119203));
#8329=CARTESIAN_POINT('Ctrl Pts',(0.750785745543687,-0.232861760990032,
0.631684198665439));
#8330=CARTESIAN_POINT('Ctrl Pts',(0.763642258217232,-0.224161999508995,
0.615966552324775));
#8331=CARTESIAN_POINT('Ctrl Pts',(0.78555112003688,-0.203463743702801,0.587792702767295));
#8332=CARTESIAN_POINT('Ctrl Pts',(0.795684265985088,-0.190326085855194,
0.573915184558108));
#8333=CARTESIAN_POINT('Ctrl Pts',(0.813159949759,-0.15976606450048,0.548874290046456));
#8334=CARTESIAN_POINT('Ctrl Pts',(0.820511285096538,-0.142345102874864,
0.537715343527944));
#8335=CARTESIAN_POINT('Ctrl Pts',(0.833661031856294,-0.099930567888331,
0.517157748491653));
#8336=CARTESIAN_POINT('Ctrl Pts',(0.838633903678357,-0.0740444353928835,
0.508899795931835));
#8337=CARTESIAN_POINT('Ctrl Pts',(0.841298510752801,-0.0476299999999999,
0.504455939115715));
#8338=CARTESIAN_POINT('',(0.528110872004958,-0.04763,0.871530771444223));
#8339=CARTESIAN_POINT('Origin',(0.707106781186547,-0.04763,0.707106781186548));
#8340=CARTESIAN_POINT('',(0.871530771444223,-0.04763,0.528110872004959));
#8341=CARTESIAN_POINT('Ctrl Pts',(0.871530771444223,-0.0476300000000001,
0.528110872004958));
#8342=CARTESIAN_POINT('Ctrl Pts',(0.87014664509073,-0.0609922781173483,
0.530395067942936));
#8343=CARTESIAN_POINT('Ctrl Pts',(0.868149331745851,-0.0742967091364493,
0.533674141594226));
#8344=CARTESIAN_POINT('Ctrl Pts',(0.85981294420286,-0.115492077056649,0.54708917182331));
#8345=CARTESIAN_POINT('Ctrl Pts',(0.850993704737257,-0.141695629206859,
0.560922177770136));
#8346=CARTESIAN_POINT('Ctrl Pts',(0.830754510485543,-0.181890537957859,
0.590422647829571));
#8347=CARTESIAN_POINT('Ctrl Pts',(0.816896541396381,-0.201072148666545,
0.609616703125488));
#8348=CARTESIAN_POINT('Ctrl Pts',(0.792310597819928,-0.223955109275652,
0.641117951819998));
#8349=CARTESIAN_POINT('Ctrl Pts',(0.779109323683612,-0.232742381310829,
0.657208095763053));
#8350=CARTESIAN_POINT('Ctrl Pts',(0.750552691816206,-0.244234834628584,
0.68964083160521));
#8351=CARTESIAN_POINT('Ctrl Pts',(0.735185187071673,-0.246942143572133,
0.705971972091755));
#8352=CARTESIAN_POINT('Ctrl Pts',(0.705971972091754,-0.246942143572133,
0.735185187071673));
#8353=CARTESIAN_POINT('Ctrl Pts',(0.689640831605209,-0.244234834628584,
0.750552691816206));
#8354=CARTESIAN_POINT('Ctrl Pts',(0.657208095763052,-0.232742381310829,
0.779109323683612));
#8355=CARTESIAN_POINT('Ctrl Pts',(0.641117951819998,-0.223955109275652,
0.792310597819928));
#8356=CARTESIAN_POINT('Ctrl Pts',(0.609616703125487,-0.201072148666545,
0.816896541396382));
#8357=CARTESIAN_POINT('Ctrl Pts',(0.590422647829571,-0.181890537957858,
0.830754510485544));
#8358=CARTESIAN_POINT('Ctrl Pts',(0.560922177770135,-0.141695629206858,
0.850993704737257));
#8359=CARTESIAN_POINT('Ctrl Pts',(0.547089171823309,-0.115492077056649,
0.859812944202861));
#8360=CARTESIAN_POINT('Ctrl Pts',(0.533674141594226,-0.0742967091364491,
0.868149331745852));
#8361=CARTESIAN_POINT('Ctrl Pts',(0.530395067942936,-0.0609922781173483,
0.870146645090731));
#8362=CARTESIAN_POINT('Ctrl Pts',(0.528110872004958,-0.0476300000000001,
0.871530771444223));
#8363=CARTESIAN_POINT('Origin',(0.707106781186547,-0.04763,0.707106781186548));
#8364=CARTESIAN_POINT('Origin',(0.,-0.166705,0.));
#8365=CARTESIAN_POINT('',(0.242834539687906,-0.04763,0.989696097314));
#8366=CARTESIAN_POINT('Origin',(0.,-0.04763,0.));
#8367=CARTESIAN_POINT('',(-0.242834539687907,-0.04763,0.989696097314));
#8368=CARTESIAN_POINT('Ctrl Pts',(0.242834539687906,-0.04763,0.989696097314));
#8369=CARTESIAN_POINT('Ctrl Pts',(0.24024064412003,-0.0609922781173483,
0.990332542620729));
#8370=CARTESIAN_POINT('Ctrl Pts',(0.236509675094874,-0.0742967091364492,
0.991238884025248));
#8371=CARTESIAN_POINT('Ctrl Pts',(0.221129100087819,-0.115492077056649,
0.994830026707808));
#8372=CARTESIAN_POINT('Ctrl Pts',(0.205111543747588,-0.141695629206859,
0.998375294985966));
#8373=CARTESIAN_POINT('Ctrl Pts',(0.169940289819232,-0.181890537957859,
1.00492400591205));
#8374=CARTESIAN_POINT('Ctrl Pts',(0.1465689792446,-0.201072148666545,1.00869718865384));
#8375=CARTESIAN_POINT('Ctrl Pts',(0.106909345252087,-0.223955109275652,
1.01358704779679));
#8376=CARTESIAN_POINT('Ctrl Pts',(0.0861971848975941,-0.232742381310829,
1.0156297872271));
#8377=CARTESIAN_POINT('Ctrl Pts',(0.0430711894098822,-0.244234834628584,
1.01837060663223));
#8378=CARTESIAN_POINT('Ctrl Pts',(0.0206568624125605,-0.246942143572133,
1.019052));
#8379=CARTESIAN_POINT('Ctrl Pts',(-0.0206568624125608,-0.246942143572133,
1.019052));
#8380=CARTESIAN_POINT('Ctrl Pts',(-0.0430711894098825,-0.244234834628584,
1.01837060663223));
#8381=CARTESIAN_POINT('Ctrl Pts',(-0.0861971848975943,-0.232742381310829,
1.0156297872271));
#8382=CARTESIAN_POINT('Ctrl Pts',(-0.106909345252088,-0.223955109275652,
1.01358704779679));
#8383=CARTESIAN_POINT('Ctrl Pts',(-0.1465689792446,-0.201072148666545,1.00869718865384));
#8384=CARTESIAN_POINT('Ctrl Pts',(-0.169940289819232,-0.181890537957859,
1.00492400591205));
#8385=CARTESIAN_POINT('Ctrl Pts',(-0.205111543747588,-0.141695629206859,
0.998375294985966));
#8386=CARTESIAN_POINT('Ctrl Pts',(-0.221129100087819,-0.115492077056649,
0.994830026707808));
#8387=CARTESIAN_POINT('Ctrl Pts',(-0.236509675094875,-0.0742967091364493,
0.991238884025248));
#8388=CARTESIAN_POINT('Ctrl Pts',(-0.24024064412003,-0.0609922781173483,
0.990332542620729));
#8389=CARTESIAN_POINT('Ctrl Pts',(-0.242834539687907,-0.04763,0.989696097314));
#8390=CARTESIAN_POINT('',(-0.528110872004959,-0.04763,0.871530771444223));
#8391=CARTESIAN_POINT('Origin',(0.,-0.04763,0.));
#8392=CARTESIAN_POINT('',(-0.871530771444223,-0.04763,0.528110872004958));
#8393=CARTESIAN_POINT('Ctrl Pts',(-0.528110872004958,-0.0476300000000001,
0.871530771444223));
#8394=CARTESIAN_POINT('Ctrl Pts',(-0.530395067942936,-0.0609922781173484,
0.87014664509073));
#8395=CARTESIAN_POINT('Ctrl Pts',(-0.533674141594226,-0.0742967091364493,
0.868149331745851));
#8396=CARTESIAN_POINT('Ctrl Pts',(-0.54708917182331,-0.115492077056649,
0.85981294420286));
#8397=CARTESIAN_POINT('Ctrl Pts',(-0.560922177770136,-0.141695629206859,
0.850993704737257));
#8398=CARTESIAN_POINT('Ctrl Pts',(-0.590422647829571,-0.181890537957859,
0.830754510485543));
#8399=CARTESIAN_POINT('Ctrl Pts',(-0.609616703125488,-0.201072148666545,
0.816896541396381));
#8400=CARTESIAN_POINT('Ctrl Pts',(-0.641117951819998,-0.223955109275652,
0.792310597819928));
#8401=CARTESIAN_POINT('Ctrl Pts',(-0.657208095763053,-0.232742381310829,
0.779109323683611));
#8402=CARTESIAN_POINT('Ctrl Pts',(-0.68964083160521,-0.244234834628584,
0.750552691816205));
#8403=CARTESIAN_POINT('Ctrl Pts',(-0.705971972091755,-0.246942143572133,
0.735185187071673));
#8404=CARTESIAN_POINT('Ctrl Pts',(-0.735185187071673,-0.246942143572133,
0.705971972091754));
#8405=CARTESIAN_POINT('Ctrl Pts',(-0.750552691816206,-0.244234834628584,
0.689640831605209));
#8406=CARTESIAN_POINT('Ctrl Pts',(-0.779109323683612,-0.232742381310829,
0.657208095763052));
#8407=CARTESIAN_POINT('Ctrl Pts',(-0.792310597819928,-0.223955109275652,
0.641117951819998));
#8408=CARTESIAN_POINT('Ctrl Pts',(-0.816896541396382,-0.201072148666545,
0.609616703125487));
#8409=CARTESIAN_POINT('Ctrl Pts',(-0.830754510485544,-0.181890537957858,
0.590422647829571));
#8410=CARTESIAN_POINT('Ctrl Pts',(-0.850993704737257,-0.141695629206858,
0.560922177770135));
#8411=CARTESIAN_POINT('Ctrl Pts',(-0.859812944202861,-0.115492077056649,
0.547089171823309));
#8412=CARTESIAN_POINT('Ctrl Pts',(-0.868149331745852,-0.0742967091364491,
0.533674141594226));
#8413=CARTESIAN_POINT('Ctrl Pts',(-0.870146645090731,-0.0609922781173483,
0.530395067942936));
#8414=CARTESIAN_POINT('Ctrl Pts',(-0.871530771444223,-0.04763,0.528110872004958));
#8415=CARTESIAN_POINT('',(-0.989696097314,-0.04763,0.242834539687906));
#8416=CARTESIAN_POINT('Origin',(0.,-0.04763,0.));
#8417=CARTESIAN_POINT('',(-1.019052,-0.246942143572133,1.248489836334E-16));
#8418=CARTESIAN_POINT('Ctrl Pts',(-0.989696097314,-0.04763,0.242834539687906));
#8419=CARTESIAN_POINT('Ctrl Pts',(-0.990332542620729,-0.0609922781173483,
0.24024064412003));
#8420=CARTESIAN_POINT('Ctrl Pts',(-0.991238884025248,-0.0742967091364492,
0.236509675094874));
#8421=CARTESIAN_POINT('Ctrl Pts',(-0.994830026707808,-0.115492077056649,
0.221129100087819));
#8422=CARTESIAN_POINT('Ctrl Pts',(-0.998375294985966,-0.141695629206859,
0.205111543747588));
#8423=CARTESIAN_POINT('Ctrl Pts',(-1.00492400591205,-0.181890537957859,
0.169940289819232));
#8424=CARTESIAN_POINT('Ctrl Pts',(-1.00869718865384,-0.201072148666545,
0.1465689792446));
#8425=CARTESIAN_POINT('Ctrl Pts',(-1.01358704779679,-0.223955109275652,
0.106909345252088));
#8426=CARTESIAN_POINT('Ctrl Pts',(-1.0156297872271,-0.232742381310829,0.0861971848975944));
#8427=CARTESIAN_POINT('Ctrl Pts',(-1.01837060663223,-0.244234834628584,
0.0430711894098825));
#8428=CARTESIAN_POINT('Ctrl Pts',(-1.019052,-0.246942143572133,0.0206568624125608));
#8429=CARTESIAN_POINT('Ctrl Pts',(-1.019052,-0.246942143572133,1.2490009027033E-16));
#8430=CARTESIAN_POINT('',(-1.019052,-0.28578,1.24797876996471E-16));
#8431=CARTESIAN_POINT('',(-1.019052,-0.166705,1.24797876996471E-16));
#8432=CARTESIAN_POINT('Origin',(0.,-0.28578,0.));
#8433=CARTESIAN_POINT('',(-0.989696097314,-0.04763,-0.242834539687906));
#8434=CARTESIAN_POINT('Ctrl Pts',(-1.019052,-0.246942143572133,1.2490009027033E-16));
#8435=CARTESIAN_POINT('Ctrl Pts',(-1.019052,-0.246942143572133,-0.0206568624125605));
#8436=CARTESIAN_POINT('Ctrl Pts',(-1.01837060663223,-0.244234834628584,
-0.0430711894098822));
#8437=CARTESIAN_POINT('Ctrl Pts',(-1.0156297872271,-0.232742381310829,-0.0861971848975941));
#8438=CARTESIAN_POINT('Ctrl Pts',(-1.01358704779679,-0.223955109275652,
-0.106909345252087));
#8439=CARTESIAN_POINT('Ctrl Pts',(-1.00869718865384,-0.201072148666546,
-0.1465689792446));
#8440=CARTESIAN_POINT('Ctrl Pts',(-1.00492400591205,-0.181890537957859,
-0.169940289819232));
#8441=CARTESIAN_POINT('Ctrl Pts',(-0.998375294985966,-0.141695629206859,
-0.205111543747588));
#8442=CARTESIAN_POINT('Ctrl Pts',(-0.994830026707808,-0.11549207705665,
-0.221129100087819));
#8443=CARTESIAN_POINT('Ctrl Pts',(-0.991238884025248,-0.0742967091364495,
-0.236509675094874));
#8444=CARTESIAN_POINT('Ctrl Pts',(-0.990332542620729,-0.0609922781173484,
-0.24024064412003));
#8445=CARTESIAN_POINT('Ctrl Pts',(-0.989696097314,-0.0476300000000001,-0.242834539687907));
#8446=CARTESIAN_POINT('',(-0.871530771444223,-0.04763,-0.528110872004958));
#8447=CARTESIAN_POINT('Origin',(0.,-0.04763,0.));
#8448=CARTESIAN_POINT('',(-0.528110872004958,-0.04763,-0.871530771444223));
#8449=CARTESIAN_POINT('Ctrl Pts',(-0.871530771444223,-0.0476300000000001,
-0.528110872004958));
#8450=CARTESIAN_POINT('Ctrl Pts',(-0.87014664509073,-0.0609922781173484,
-0.530395067942936));
#8451=CARTESIAN_POINT('Ctrl Pts',(-0.868149331745851,-0.0742967091364494,
-0.533674141594226));
#8452=CARTESIAN_POINT('Ctrl Pts',(-0.85981294420286,-0.115492077056649,
-0.54708917182331));
#8453=CARTESIAN_POINT('Ctrl Pts',(-0.850993704737257,-0.141695629206859,
-0.560922177770136));
#8454=CARTESIAN_POINT('Ctrl Pts',(-0.830754510485543,-0.181890537957859,
-0.590422647829571));
#8455=CARTESIAN_POINT('Ctrl Pts',(-0.816896541396381,-0.201072148666546,
-0.609616703125488));
#8456=CARTESIAN_POINT('Ctrl Pts',(-0.792310597819928,-0.223955109275652,
-0.641117951819999));
#8457=CARTESIAN_POINT('Ctrl Pts',(-0.779109323683611,-0.232742381310829,
-0.657208095763053));
#8458=CARTESIAN_POINT('Ctrl Pts',(-0.750552691816205,-0.244234834628584,
-0.68964083160521));
#8459=CARTESIAN_POINT('Ctrl Pts',(-0.735185187071673,-0.246942143572133,
-0.705971972091755));
#8460=CARTESIAN_POINT('Ctrl Pts',(-0.705971972091754,-0.246942143572133,
-0.735185187071673));
#8461=CARTESIAN_POINT('Ctrl Pts',(-0.68964083160521,-0.244234834628584,
-0.750552691816206));
#8462=CARTESIAN_POINT('Ctrl Pts',(-0.657208095763052,-0.232742381310829,
-0.779109323683612));
#8463=CARTESIAN_POINT('Ctrl Pts',(-0.641117951819998,-0.223955109275652,
-0.792310597819928));
#8464=CARTESIAN_POINT('Ctrl Pts',(-0.609616703125488,-0.201072148666545,
-0.816896541396381));
#8465=CARTESIAN_POINT('Ctrl Pts',(-0.590422647829571,-0.181890537957859,
-0.830754510485543));
#8466=CARTESIAN_POINT('Ctrl Pts',(-0.560922177770136,-0.141695629206859,
-0.850993704737257));
#8467=CARTESIAN_POINT('Ctrl Pts',(-0.54708917182331,-0.115492077056649,
-0.85981294420286));
#8468=CARTESIAN_POINT('Ctrl Pts',(-0.533674141594226,-0.0742967091364494,
-0.868149331745852));
#8469=CARTESIAN_POINT('Ctrl Pts',(-0.530395067942936,-0.0609922781173484,
-0.870146645090731));
#8470=CARTESIAN_POINT('Ctrl Pts',(-0.528110872004958,-0.0476300000000001,
-0.871530771444223));
#8471=CARTESIAN_POINT('',(-0.242834539687906,-0.04763,-0.989696097314));
#8472=CARTESIAN_POINT('Origin',(0.,-0.04763,0.));
#8473=CARTESIAN_POINT('',(0.242834539687906,-0.04763,-0.989696097314));
#8474=CARTESIAN_POINT('Ctrl Pts',(-0.242834539687907,-0.04763,-0.989696097314));
#8475=CARTESIAN_POINT('Ctrl Pts',(-0.24024064412003,-0.0609922781173483,
-0.990332542620729));
#8476=CARTESIAN_POINT('Ctrl Pts',(-0.236509675094874,-0.0742967091364493,
-0.991238884025248));
#8477=CARTESIAN_POINT('Ctrl Pts',(-0.221129100087819,-0.115492077056649,
-0.994830026707808));
#8478=CARTESIAN_POINT('Ctrl Pts',(-0.205111543747588,-0.141695629206859,
-0.998375294985966));
#8479=CARTESIAN_POINT('Ctrl Pts',(-0.169940289819232,-0.181890537957859,
-1.00492400591205));
#8480=CARTESIAN_POINT('Ctrl Pts',(-0.1465689792446,-0.201072148666545,-1.00869718865384));
#8481=CARTESIAN_POINT('Ctrl Pts',(-0.106909345252087,-0.223955109275652,
-1.01358704779679));
#8482=CARTESIAN_POINT('Ctrl Pts',(-0.0861971848975942,-0.232742381310829,
-1.0156297872271));
#8483=CARTESIAN_POINT('Ctrl Pts',(-0.0430711894098823,-0.244234834628584,
-1.01837060663223));
#8484=CARTESIAN_POINT('Ctrl Pts',(-0.0206568624125606,-0.246942143572133,
-1.019052));
#8485=CARTESIAN_POINT('Ctrl Pts',(0.0206568624125607,-0.246942143572133,
-1.019052));
#8486=CARTESIAN_POINT('Ctrl Pts',(0.0430711894098824,-0.244234834628584,
-1.01837060663223));
#8487=CARTESIAN_POINT('Ctrl Pts',(0.0861971848975943,-0.232742381310829,
-1.0156297872271));
#8488=CARTESIAN_POINT('Ctrl Pts',(0.106909345252088,-0.223955109275652,
-1.01358704779679));
#8489=CARTESIAN_POINT('Ctrl Pts',(0.1465689792446,-0.201072148666545,-1.00869718865384));
#8490=CARTESIAN_POINT('Ctrl Pts',(0.169940289819232,-0.181890537957859,
-1.00492400591205));
#8491=CARTESIAN_POINT('Ctrl Pts',(0.205111543747588,-0.141695629206859,
-0.998375294985966));
#8492=CARTESIAN_POINT('Ctrl Pts',(0.221129100087819,-0.115492077056649,
-0.994830026707808));
#8493=CARTESIAN_POINT('Ctrl Pts',(0.236509675094874,-0.0742967091364493,
-0.991238884025248));
#8494=CARTESIAN_POINT('Ctrl Pts',(0.24024064412003,-0.0609922781173484,
-0.990332542620729));
#8495=CARTESIAN_POINT('Ctrl Pts',(0.242834539687907,-0.04763,-0.989696097314));
#8496=CARTESIAN_POINT('',(0.528110872004958,-0.04763,-0.871530771444223));
#8497=CARTESIAN_POINT('Origin',(0.,-0.04763,0.));
#8498=CARTESIAN_POINT('',(0.871530771444223,-0.04763,-0.528110872004958));
#8499=CARTESIAN_POINT('Ctrl Pts',(0.528110872004958,-0.0476300000000001,
-0.871530771444223));
#8500=CARTESIAN_POINT('Ctrl Pts',(0.530395067942936,-0.0609922781173484,
-0.870146645090731));
#8501=CARTESIAN_POINT('Ctrl Pts',(0.533674141594226,-0.0742967091364493,
-0.868149331745851));
#8502=CARTESIAN_POINT('Ctrl Pts',(0.54708917182331,-0.115492077056649,-0.85981294420286));
#8503=CARTESIAN_POINT('Ctrl Pts',(0.560922177770136,-0.141695629206859,
-0.850993704737257));
#8504=CARTESIAN_POINT('Ctrl Pts',(0.590422647829571,-0.181890537957859,
-0.830754510485543));
#8505=CARTESIAN_POINT('Ctrl Pts',(0.609616703125488,-0.201072148666545,
-0.816896541396381));
#8506=CARTESIAN_POINT('Ctrl Pts',(0.641117951819998,-0.223955109275652,
-0.792310597819928));
#8507=CARTESIAN_POINT('Ctrl Pts',(0.657208095763053,-0.232742381310829,
-0.779109323683612));
#8508=CARTESIAN_POINT('Ctrl Pts',(0.68964083160521,-0.244234834628584,-0.750552691816206));
#8509=CARTESIAN_POINT('Ctrl Pts',(0.705971972091755,-0.246942143572133,
-0.735185187071673));
#8510=CARTESIAN_POINT('Ctrl Pts',(0.735185187071673,-0.246942143572133,
-0.705971972091754));
#8511=CARTESIAN_POINT('Ctrl Pts',(0.750552691816206,-0.244234834628584,
-0.68964083160521));
#8512=CARTESIAN_POINT('Ctrl Pts',(0.779109323683612,-0.232742381310829,
-0.657208095763053));
#8513=CARTESIAN_POINT('Ctrl Pts',(0.792310597819928,-0.223955109275652,
-0.641117951819998));
#8514=CARTESIAN_POINT('Ctrl Pts',(0.816896541396381,-0.201072148666545,
-0.609616703125488));
#8515=CARTESIAN_POINT('Ctrl Pts',(0.830754510485543,-0.181890537957859,
-0.590422647829571));
#8516=CARTESIAN_POINT('Ctrl Pts',(0.850993704737257,-0.141695629206859,
-0.560922177770136));
#8517=CARTESIAN_POINT('Ctrl Pts',(0.85981294420286,-0.115492077056649,-0.54708917182331));
#8518=CARTESIAN_POINT('Ctrl Pts',(0.868149331745851,-0.0742967091364493,
-0.533674141594226));
#8519=CARTESIAN_POINT('Ctrl Pts',(0.870146645090731,-0.0609922781173484,
-0.530395067942936));
#8520=CARTESIAN_POINT('Ctrl Pts',(0.871530771444223,-0.0476300000000001,
-0.528110872004958));
#8521=CARTESIAN_POINT('',(0.989696097314,-0.04763,-0.242834539687906));
#8522=CARTESIAN_POINT('Origin',(0.,-0.04763,0.));
#8523=CARTESIAN_POINT('',(0.989696097314,-0.04763,0.242834539687906));
#8524=CARTESIAN_POINT('Ctrl Pts',(0.989696097314,-0.04763,-0.242834539687907));
#8525=CARTESIAN_POINT('Ctrl Pts',(0.990332542620729,-0.0609922781173483,
-0.24024064412003));
#8526=CARTESIAN_POINT('Ctrl Pts',(0.991238884025248,-0.0742967091364493,
-0.236509675094874));
#8527=CARTESIAN_POINT('Ctrl Pts',(0.994830026707808,-0.115492077056649,
-0.221129100087819));
#8528=CARTESIAN_POINT('Ctrl Pts',(0.998375294985966,-0.141695629206859,
-0.205111543747588));
#8529=CARTESIAN_POINT('Ctrl Pts',(1.00492400591205,-0.181890537957859,-0.169940289819232));
#8530=CARTESIAN_POINT('Ctrl Pts',(1.00869718865384,-0.201072148666545,-0.1465689792446));
#8531=CARTESIAN_POINT('Ctrl Pts',(1.01358704779679,-0.223955109275652,-0.106909345252087));
#8532=CARTESIAN_POINT('Ctrl Pts',(1.0156297872271,-0.232742381310829,-0.0861971848975942));
#8533=CARTESIAN_POINT('Ctrl Pts',(1.01837060663223,-0.244234834628584,-0.0430711894098823));
#8534=CARTESIAN_POINT('Ctrl Pts',(1.019052,-0.246942143572133,-0.0206568624125607));
#8535=CARTESIAN_POINT('Ctrl Pts',(1.019052,-0.246942143572133,0.0206568624125607));
#8536=CARTESIAN_POINT('Ctrl Pts',(1.01837060663223,-0.244234834628584,0.0430711894098823));
#8537=CARTESIAN_POINT('Ctrl Pts',(1.0156297872271,-0.232742381310829,0.0861971848975942));
#8538=CARTESIAN_POINT('Ctrl Pts',(1.01358704779679,-0.223955109275652,0.106909345252087));
#8539=CARTESIAN_POINT('Ctrl Pts',(1.00869718865384,-0.201072148666545,0.1465689792446));
#8540=CARTESIAN_POINT('Ctrl Pts',(1.00492400591205,-0.181890537957859,0.169940289819232));
#8541=CARTESIAN_POINT('Ctrl Pts',(0.998375294985966,-0.141695629206859,
0.205111543747588));
#8542=CARTESIAN_POINT('Ctrl Pts',(0.994830026707808,-0.115492077056649,
0.221129100087819));
#8543=CARTESIAN_POINT('Ctrl Pts',(0.991238884025248,-0.0742967091364492,
0.236509675094874));
#8544=CARTESIAN_POINT('Ctrl Pts',(0.990332542620729,-0.0609922781173483,
0.24024064412003));
#8545=CARTESIAN_POINT('Ctrl Pts',(0.989696097314,-0.04763,0.242834539687907));
#8546=CARTESIAN_POINT('Origin',(0.,-0.04763,0.));
#8547=CARTESIAN_POINT('Origin',(0.,-0.04763,0.));
#8548=CARTESIAN_POINT('',(0.238183666596899,-0.04763,0.951592097314));
#8549=CARTESIAN_POINT('Origin',(0.,-0.04763,0.));
#8550=CARTESIAN_POINT('Origin',(-1.94289029309402E-16,-0.04763,1.));
#8551=CARTESIAN_POINT('Origin',(-1.94289029309402E-16,0.,1.));
#8552=CARTESIAN_POINT('',(-0.2381836665969,-0.04763,0.951592097314));
#8553=CARTESIAN_POINT('Ctrl Pts',(-0.238183666596899,-0.0476299999999999,
0.951592097314));
#8554=CARTESIAN_POINT('Ctrl Pts',(-0.233157223576062,-0.0740444353928835,
0.952850216871763));
#8555=CARTESIAN_POINT('Ctrl Pts',(-0.223801617934946,-0.0999305678883309,
0.955173119738174));
#8556=CARTESIAN_POINT('Ctrl Pts',(-0.199966927975188,-0.142345102874864,
0.960411259488514));
#8557=CARTESIAN_POINT('Ctrl Pts',(-0.1868781821531,-0.159766064500479,0.963103647174702));
#8558=CARTESIAN_POINT('Ctrl Pts',(-0.15681442133453,-0.190326085855194,
0.968453058988463));
#8559=CARTESIAN_POINT('Ctrl Pts',(-0.139836317888043,-0.203463743702801,
0.971100730005489));
#8560=CARTESIAN_POINT('Ctrl Pts',(-0.104422493053067,-0.224161999508995,
0.975530745318961));
#8561=CARTESIAN_POINT('Ctrl Pts',(-0.0842175114474176,-0.232861760990032,
0.977553872336861));
#8562=CARTESIAN_POINT('Ctrl Pts',(-0.0421062857595701,-0.244251601209411,
0.980270995488453));
#8563=CARTESIAN_POINT('Ctrl Pts',(-0.0201990724523197,-0.246942143572133,
0.980948));
#8564=CARTESIAN_POINT('Ctrl Pts',(0.020199072452319,-0.246942143572133,
0.980948));
#8565=CARTESIAN_POINT('Ctrl Pts',(0.0421062857595694,-0.244251601209411,
0.980270995488454));
#8566=CARTESIAN_POINT('Ctrl Pts',(0.0842175114474169,-0.232861760990032,
0.977553872336861));
#8567=CARTESIAN_POINT('Ctrl Pts',(0.104422493053067,-0.224161999508995,
0.975530745318961));
#8568=CARTESIAN_POINT('Ctrl Pts',(0.139836317888042,-0.203463743702801,
0.971100730005489));
#8569=CARTESIAN_POINT('Ctrl Pts',(0.15681442133453,-0.190326085855194,0.968453058988463));
#8570=CARTESIAN_POINT('Ctrl Pts',(0.1868781821531,-0.15976606450048,0.963103647174702));
#8571=CARTESIAN_POINT('Ctrl Pts',(0.199966927975188,-0.142345102874864,
0.960411259488514));
#8572=CARTESIAN_POINT('Ctrl Pts',(0.223801617934945,-0.0999305678883309,
0.955173119738174));
#8573=CARTESIAN_POINT('Ctrl Pts',(0.233157223576061,-0.0740444353928835,
0.952850216871763));
#8574=CARTESIAN_POINT('Ctrl Pts',(0.238183666596899,-0.0476299999999999,
0.951592097314));
#8575=CARTESIAN_POINT('Origin',(-1.94289029309402E-16,-0.04763,1.));
#8576=CARTESIAN_POINT('Origin',(0.,-0.04763,0.));
#8577=CARTESIAN_POINT('',(-0.504455939115715,-0.04763,0.841298510752802));
#8578=CARTESIAN_POINT('Origin',(0.,-0.04763,0.));
#8579=CARTESIAN_POINT('Origin',(-0.707106781186548,-0.04763,0.707106781186547));
#8580=CARTESIAN_POINT('Origin',(-0.707106781186548,0.,0.707106781186547));
#8581=CARTESIAN_POINT('',(-0.841298510752802,-0.04763,0.504455939115715));
#8582=CARTESIAN_POINT('Ctrl Pts',(-0.841298510752802,-0.04763,0.504455939115715));
#8583=CARTESIAN_POINT('Ctrl Pts',(-0.838633903678357,-0.0740444353928835,
0.508899795931835));
#8584=CARTESIAN_POINT('Ctrl Pts',(-0.833661031856294,-0.0999305678883309,
0.517157748491652));
#8585=CARTESIAN_POINT('Ctrl Pts',(-0.820511285096538,-0.142345102874864,
0.537715343527944));
#8586=CARTESIAN_POINT('Ctrl Pts',(-0.813159949759,-0.159766064500479,0.548874290046456));
#8587=CARTESIAN_POINT('Ctrl Pts',(-0.795684265985089,-0.190326085855194,
0.573915184558107));
#8588=CARTESIAN_POINT('Ctrl Pts',(-0.78555112003688,-0.203463743702801,
0.587792702767295));
#8589=CARTESIAN_POINT('Ctrl Pts',(-0.763642258217233,-0.224161999508995,
0.615966552324775));
#8590=CARTESIAN_POINT('Ctrl Pts',(-0.750785745543687,-0.232861760990032,
0.631684198665438));
#8591=CARTESIAN_POINT('Ctrl Pts',(-0.722929908501543,-0.244251601209411,
0.663382628119203));
#8592=CARTESIAN_POINT('Ctrl Pts',(-0.707917883896095,-0.246942143572133,
0.679352081686668));
#8593=CARTESIAN_POINT('Ctrl Pts',(-0.679352081686668,-0.246942143572133,
0.707917883896095));
#8594=CARTESIAN_POINT('Ctrl Pts',(-0.663382628119203,-0.244251601209411,
0.722929908501544));
#8595=CARTESIAN_POINT('Ctrl Pts',(-0.631684198665438,-0.232861760990031,
0.750785745543687));
#8596=CARTESIAN_POINT('Ctrl Pts',(-0.615966552324775,-0.224161999508995,
0.763642258217233));
#8597=CARTESIAN_POINT('Ctrl Pts',(-0.587792702767295,-0.203463743702801,
0.78555112003688));
#8598=CARTESIAN_POINT('Ctrl Pts',(-0.573915184558107,-0.190326085855194,
0.795684265985088));
#8599=CARTESIAN_POINT('Ctrl Pts',(-0.548874290046456,-0.159766064500479,
0.813159949759));
#8600=CARTESIAN_POINT('Ctrl Pts',(-0.537715343527944,-0.142345102874864,
0.820511285096538));
#8601=CARTESIAN_POINT('Ctrl Pts',(-0.517157748491652,-0.0999305678883309,
0.833661031856294));
#8602=CARTESIAN_POINT('Ctrl Pts',(-0.508899795931835,-0.0740444353928835,
0.838633903678357));
#8603=CARTESIAN_POINT('Ctrl Pts',(-0.504455939115716,-0.04763,0.841298510752801));
#8604=CARTESIAN_POINT('Origin',(-0.707106781186548,-0.04763,0.707106781186547));
#8605=CARTESIAN_POINT('Origin',(0.,-0.04763,0.));
#8606=CARTESIAN_POINT('',(-0.951592097314,-0.04763,0.238183666596899));
#8607=CARTESIAN_POINT('Origin',(0.,-0.04763,0.));
#8608=CARTESIAN_POINT('Origin',(-1.,-0.04763,-1.11022302462516E-16));
#8609=CARTESIAN_POINT('Origin',(-1.,0.,-1.11022302462516E-16));
#8610=CARTESIAN_POINT('',(-0.951592097314,-0.04763,-0.2381836665969));
#8611=CARTESIAN_POINT('',(-0.980948,-0.246942143572133,1.08514323328844E-18));
#8612=CARTESIAN_POINT('Ctrl Pts',(-0.951592097314,-0.04763,-0.238183666596899));
#8613=CARTESIAN_POINT('Ctrl Pts',(-0.952850216871763,-0.0740444353928835,
-0.233157223576062));
#8614=CARTESIAN_POINT('Ctrl Pts',(-0.955173119738174,-0.0999305678883309,
-0.223801617934946));
#8615=CARTESIAN_POINT('Ctrl Pts',(-0.960411259488514,-0.142345102874864,
-0.199966927975188));
#8616=CARTESIAN_POINT('Ctrl Pts',(-0.963103647174702,-0.159766064500479,
-0.1868781821531));
#8617=CARTESIAN_POINT('Ctrl Pts',(-0.968453058988463,-0.190326085855194,
-0.15681442133453));
#8618=CARTESIAN_POINT('Ctrl Pts',(-0.971100730005489,-0.203463743702801,
-0.139836317888043));
#8619=CARTESIAN_POINT('Ctrl Pts',(-0.975530745318961,-0.224161999508995,
-0.104422493053067));
#8620=CARTESIAN_POINT('Ctrl Pts',(-0.977553872336861,-0.232861760990032,
-0.0842175114474175));
#8621=CARTESIAN_POINT('Ctrl Pts',(-0.980270995488453,-0.244251601209411,
-0.0421062857595699));
#8622=CARTESIAN_POINT('Ctrl Pts',(-0.980948,-0.246942143572133,-0.0201990724523195));
#8623=CARTESIAN_POINT('Ctrl Pts',(-0.980948,-0.246942143572133,-1.17961196366423E-16));
#8624=CARTESIAN_POINT('Origin',(-1.,-0.04763,-1.11022302462516E-16));
#8625=CARTESIAN_POINT('Ctrl Pts',(-0.980948,-0.246942143572133,-1.17961196366423E-16));
#8626=CARTESIAN_POINT('Ctrl Pts',(-0.980948,-0.246942143572133,0.0201990724523192));
#8627=CARTESIAN_POINT('Ctrl Pts',(-0.980270995488453,-0.244251601209411,
0.0421062857595695));
#8628=CARTESIAN_POINT('Ctrl Pts',(-0.977553872336861,-0.232861760990032,
0.0842175114474169));
#8629=CARTESIAN_POINT('Ctrl Pts',(-0.975530745318961,-0.224161999508995,
0.104422493053066));
#8630=CARTESIAN_POINT('Ctrl Pts',(-0.971100730005489,-0.203463743702801,
0.139836317888042));
#8631=CARTESIAN_POINT('Ctrl Pts',(-0.968453058988463,-0.190326085855194,
0.15681442133453));
#8632=CARTESIAN_POINT('Ctrl Pts',(-0.963103647174702,-0.15976606450048,
0.1868781821531));
#8633=CARTESIAN_POINT('Ctrl Pts',(-0.960411259488514,-0.142345102874864,
0.199966927975188));
#8634=CARTESIAN_POINT('Ctrl Pts',(-0.955173119738174,-0.099930567888331,
0.223801617934945));
#8635=CARTESIAN_POINT('Ctrl Pts',(-0.952850216871763,-0.0740444353928835,
0.233157223576061));
#8636=CARTESIAN_POINT('Ctrl Pts',(-0.951592097314,-0.04763,0.238183666596899));
#8637=CARTESIAN_POINT('Origin',(0.,-0.04763,0.));
#8638=CARTESIAN_POINT('',(-0.841298510752802,-0.04763,-0.504455939115715));
#8639=CARTESIAN_POINT('Origin',(0.,-0.04763,0.));
#8640=CARTESIAN_POINT('Origin',(-0.707106781186547,-0.04763,-0.707106781186548));
#8641=CARTESIAN_POINT('Origin',(-0.707106781186547,0.,-0.707106781186548));
#8642=CARTESIAN_POINT('',(-0.504455939115715,-0.04763,-0.841298510752802));
#8643=CARTESIAN_POINT('Ctrl Pts',(-0.504455939115715,-0.04763,-0.841298510752802));
#8644=CARTESIAN_POINT('Ctrl Pts',(-0.508899795931835,-0.0740444353928835,
-0.838633903678357));
#8645=CARTESIAN_POINT('Ctrl Pts',(-0.517157748491652,-0.0999305678883309,
-0.833661031856294));
#8646=CARTESIAN_POINT('Ctrl Pts',(-0.537715343527944,-0.142345102874864,
-0.820511285096538));
#8647=CARTESIAN_POINT('Ctrl Pts',(-0.548874290046456,-0.159766064500479,
-0.813159949759));
#8648=CARTESIAN_POINT('Ctrl Pts',(-0.573915184558107,-0.190326085855194,
-0.795684265985089));
#8649=CARTESIAN_POINT('Ctrl Pts',(-0.587792702767295,-0.203463743702801,
-0.78555112003688));
#8650=CARTESIAN_POINT('Ctrl Pts',(-0.615966552324775,-0.224161999508995,
-0.763642258217233));
#8651=CARTESIAN_POINT('Ctrl Pts',(-0.631684198665438,-0.232861760990032,
-0.750785745543687));
#8652=CARTESIAN_POINT('Ctrl Pts',(-0.663382628119203,-0.244251601209411,
-0.722929908501543));
#8653=CARTESIAN_POINT('Ctrl Pts',(-0.679352081686668,-0.246942143572133,
-0.707917883896095));
#8654=CARTESIAN_POINT('Ctrl Pts',(-0.707917883896095,-0.246942143572133,
-0.679352081686668));
#8655=CARTESIAN_POINT('Ctrl Pts',(-0.722929908501543,-0.244251601209411,
-0.663382628119203));
#8656=CARTESIAN_POINT('Ctrl Pts',(-0.750785745543687,-0.232861760990032,
-0.631684198665439));
#8657=CARTESIAN_POINT('Ctrl Pts',(-0.763642258217232,-0.224161999508995,
-0.615966552324775));
#8658=CARTESIAN_POINT('Ctrl Pts',(-0.78555112003688,-0.203463743702801,
-0.587792702767295));
#8659=CARTESIAN_POINT('Ctrl Pts',(-0.795684265985088,-0.190326085855194,
-0.573915184558107));
#8660=CARTESIAN_POINT('Ctrl Pts',(-0.813159949759,-0.15976606450048,-0.548874290046456));
#8661=CARTESIAN_POINT('Ctrl Pts',(-0.820511285096538,-0.142345102874864,
-0.537715343527944));
#8662=CARTESIAN_POINT('Ctrl Pts',(-0.833661031856294,-0.0999305678883311,
-0.517157748491652));
#8663=CARTESIAN_POINT('Ctrl Pts',(-0.838633903678357,-0.0740444353928836,
-0.508899795931835));
#8664=CARTESIAN_POINT('Ctrl Pts',(-0.841298510752801,-0.04763,-0.504455939115715));
#8665=CARTESIAN_POINT('Origin',(-0.707106781186547,-0.04763,-0.707106781186548));
#8666=CARTESIAN_POINT('Origin',(0.,-0.04763,0.));
#8667=CARTESIAN_POINT('',(-0.238183666596899,-0.04763,-0.951592097314));
#8668=CARTESIAN_POINT('Origin',(0.,-0.04763,0.));
#8669=CARTESIAN_POINT('Origin',(5.55111512312578E-17,-0.04763,-1.));
#8670=CARTESIAN_POINT('Origin',(5.55111512312578E-17,0.,-1.));
#8671=CARTESIAN_POINT('',(0.238183666596899,-0.04763,-0.951592097314));
#8672=CARTESIAN_POINT('Ctrl Pts',(0.238183666596899,-0.04763,-0.951592097314));
#8673=CARTESIAN_POINT('Ctrl Pts',(0.233157223576062,-0.0740444353928835,
-0.952850216871763));
#8674=CARTESIAN_POINT('Ctrl Pts',(0.223801617934946,-0.099930567888331,
-0.955173119738174));
#8675=CARTESIAN_POINT('Ctrl Pts',(0.199966927975188,-0.142345102874864,
-0.960411259488514));
#8676=CARTESIAN_POINT('Ctrl Pts',(0.1868781821531,-0.15976606450048,-0.963103647174702));
#8677=CARTESIAN_POINT('Ctrl Pts',(0.15681442133453,-0.190326085855194,-0.968453058988463));
#8678=CARTESIAN_POINT('Ctrl Pts',(0.139836317888042,-0.203463743702801,
-0.971100730005489));
#8679=CARTESIAN_POINT('Ctrl Pts',(0.104422493053067,-0.224161999508995,
-0.975530745318961));
#8680=CARTESIAN_POINT('Ctrl Pts',(0.0842175114474173,-0.232861760990032,
-0.977553872336861));
#8681=CARTESIAN_POINT('Ctrl Pts',(0.0421062857595698,-0.244251601209411,
-0.980270995488453));
#8682=CARTESIAN_POINT('Ctrl Pts',(0.0201990724523194,-0.246942143572133,
-0.980948));
#8683=CARTESIAN_POINT('Ctrl Pts',(-0.0201990724523193,-0.246942143572133,
-0.980948));
#8684=CARTESIAN_POINT('Ctrl Pts',(-0.0421062857595697,-0.244251601209411,
-0.980270995488453));
#8685=CARTESIAN_POINT('Ctrl Pts',(-0.0842175114474171,-0.232861760990032,
-0.977553872336861));
#8686=CARTESIAN_POINT('Ctrl Pts',(-0.104422493053067,-0.224161999508995,
-0.975530745318961));
#8687=CARTESIAN_POINT('Ctrl Pts',(-0.139836317888042,-0.203463743702801,
-0.971100730005489));
#8688=CARTESIAN_POINT('Ctrl Pts',(-0.15681442133453,-0.190326085855194,
-0.968453058988463));
#8689=CARTESIAN_POINT('Ctrl Pts',(-0.1868781821531,-0.15976606450048,-0.963103647174702));
#8690=CARTESIAN_POINT('Ctrl Pts',(-0.199966927975188,-0.142345102874864,
-0.960411259488514));
#8691=CARTESIAN_POINT('Ctrl Pts',(-0.223801617934945,-0.099930567888331,
-0.955173119738174));
#8692=CARTESIAN_POINT('Ctrl Pts',(-0.233157223576062,-0.0740444353928835,
-0.952850216871763));
#8693=CARTESIAN_POINT('Ctrl Pts',(-0.238183666596899,-0.0476299999999999,
-0.951592097314));
#8694=CARTESIAN_POINT('Origin',(5.55111512312578E-17,-0.04763,-1.));
#8695=CARTESIAN_POINT('Origin',(0.,-0.04763,0.));
#8696=CARTESIAN_POINT('',(0.504455939115715,-0.04763,-0.841298510752802));
#8697=CARTESIAN_POINT('Origin',(0.,-0.04763,0.));
#8698=CARTESIAN_POINT('Origin',(0.707106781186548,-0.04763,-0.707106781186547));
#8699=CARTESIAN_POINT('Origin',(0.707106781186548,0.,-0.707106781186547));
#8700=CARTESIAN_POINT('',(0.841298510752802,-0.04763,-0.504455939115715));
#8701=CARTESIAN_POINT('Ctrl Pts',(0.841298510752802,-0.04763,-0.504455939115715));
#8702=CARTESIAN_POINT('Ctrl Pts',(0.838633903678357,-0.0740444353928835,
-0.508899795931835));
#8703=CARTESIAN_POINT('Ctrl Pts',(0.833661031856294,-0.0999305678883309,
-0.517157748491652));
#8704=CARTESIAN_POINT('Ctrl Pts',(0.820511285096538,-0.142345102874864,
-0.537715343527944));
#8705=CARTESIAN_POINT('Ctrl Pts',(0.813159949759,-0.159766064500479,-0.548874290046456));
#8706=CARTESIAN_POINT('Ctrl Pts',(0.795684265985088,-0.190326085855194,
-0.573915184558107));
#8707=CARTESIAN_POINT('Ctrl Pts',(0.78555112003688,-0.203463743702801,-0.587792702767295));
#8708=CARTESIAN_POINT('Ctrl Pts',(0.763642258217233,-0.224161999508995,
-0.615966552324775));
#8709=CARTESIAN_POINT('Ctrl Pts',(0.750785745543687,-0.232861760990032,
-0.631684198665438));
#8710=CARTESIAN_POINT('Ctrl Pts',(0.722929908501543,-0.244251601209411,
-0.663382628119203));
#8711=CARTESIAN_POINT('Ctrl Pts',(0.707917883896095,-0.246942143572133,
-0.679352081686668));
#8712=CARTESIAN_POINT('Ctrl Pts',(0.679352081686668,-0.246942143572133,
-0.707917883896095));
#8713=CARTESIAN_POINT('Ctrl Pts',(0.663382628119203,-0.244251601209411,
-0.722929908501543));
#8714=CARTESIAN_POINT('Ctrl Pts',(0.631684198665438,-0.232861760990032,
-0.750785745543687));
#8715=CARTESIAN_POINT('Ctrl Pts',(0.615966552324775,-0.224161999508995,
-0.763642258217232));
#8716=CARTESIAN_POINT('Ctrl Pts',(0.587792702767295,-0.203463743702801,
-0.78555112003688));
#8717=CARTESIAN_POINT('Ctrl Pts',(0.573915184558107,-0.190326085855194,
-0.795684265985088));
#8718=CARTESIAN_POINT('Ctrl Pts',(0.548874290046456,-0.159766064500479,
-0.813159949759));
#8719=CARTESIAN_POINT('Ctrl Pts',(0.537715343527944,-0.142345102874864,
-0.820511285096538));
#8720=CARTESIAN_POINT('Ctrl Pts',(0.517157748491652,-0.099930567888331,
-0.833661031856294));
#8721=CARTESIAN_POINT('Ctrl Pts',(0.508899795931835,-0.0740444353928835,
-0.838633903678357));
#8722=CARTESIAN_POINT('Ctrl Pts',(0.504455939115715,-0.04763,-0.841298510752801));
#8723=CARTESIAN_POINT('Origin',(0.707106781186548,-0.04763,-0.707106781186547));
#8724=CARTESIAN_POINT('Origin',(0.,-0.166705,0.));
#8725=CARTESIAN_POINT('',(-0.980948,-0.28578,1.20131482833E-16));
#8726=CARTESIAN_POINT('Origin',(0.,-0.28578,0.));
#8727=CARTESIAN_POINT('',(-0.980948,-0.166705,1.20131482833E-16));
#8728=CARTESIAN_POINT('',(0.951592097314,-0.04763,0.238183666596899));
#8729=CARTESIAN_POINT('Origin',(0.,-0.04763,0.));
#8730=CARTESIAN_POINT('',(0.951592097314,-0.04763,-0.238183666596899));
#8731=CARTESIAN_POINT('Ctrl Pts',(0.951592097314,-0.04763,0.238183666596899));
#8732=CARTESIAN_POINT('Ctrl Pts',(0.952850216871763,-0.0740444353928835,
0.233157223576062));
#8733=CARTESIAN_POINT('Ctrl Pts',(0.955173119738174,-0.099930567888331,
0.223801617934945));
#8734=CARTESIAN_POINT('Ctrl Pts',(0.960411259488514,-0.142345102874864,
0.199966927975188));
#8735=CARTESIAN_POINT('Ctrl Pts',(0.963103647174702,-0.15976606450048,0.1868781821531));
#8736=CARTESIAN_POINT('Ctrl Pts',(0.968453058988463,-0.190326085855194,
0.15681442133453));
#8737=CARTESIAN_POINT('Ctrl Pts',(0.971100730005489,-0.203463743702801,
0.139836317888042));
#8738=CARTESIAN_POINT('Ctrl Pts',(0.975530745318961,-0.224161999508995,
0.104422493053067));
#8739=CARTESIAN_POINT('Ctrl Pts',(0.977553872336861,-0.232861760990032,
0.0842175114474172));
#8740=CARTESIAN_POINT('Ctrl Pts',(0.980270995488453,-0.244251601209411,
0.0421062857595697));
#8741=CARTESIAN_POINT('Ctrl Pts',(0.980948,-0.246942143572133,0.0201990724523194));
#8742=CARTESIAN_POINT('Ctrl Pts',(0.980948,-0.246942143572133,-0.0201990724523194));
#8743=CARTESIAN_POINT('Ctrl Pts',(0.980270995488453,-0.244251601209411,
-0.0421062857595697));
#8744=CARTESIAN_POINT('Ctrl Pts',(0.977553872336861,-0.232861760990032,
-0.0842175114474172));
#8745=CARTESIAN_POINT('Ctrl Pts',(0.975530745318961,-0.224161999508995,
-0.104422493053067));
#8746=CARTESIAN_POINT('Ctrl Pts',(0.971100730005489,-0.203463743702801,
-0.139836317888042));
#8747=CARTESIAN_POINT('Ctrl Pts',(0.968453058988463,-0.190326085855194,
-0.15681442133453));
#8748=CARTESIAN_POINT('Ctrl Pts',(0.963103647174702,-0.15976606450048,-0.1868781821531));
#8749=CARTESIAN_POINT('Ctrl Pts',(0.960411259488514,-0.142345102874864,
-0.199966927975188));
#8750=CARTESIAN_POINT('Ctrl Pts',(0.955173119738174,-0.099930567888331,
-0.223801617934945));
#8751=CARTESIAN_POINT('Ctrl Pts',(0.952850216871763,-0.0740444353928835,
-0.233157223576062));
#8752=CARTESIAN_POINT('Ctrl Pts',(0.951592097314,-0.0476299999999999,-0.238183666596899));
#8753=CARTESIAN_POINT('Origin',(0.,-0.04763,0.));
#8754=CARTESIAN_POINT('Origin',(0.,-0.04763,0.));
#8755=CARTESIAN_POINT('Origin',(1.,-0.04763,0.));
#8756=CARTESIAN_POINT('Origin',(1.,0.,0.));
#8757=CARTESIAN_POINT('Origin',(1.,-0.04763,0.));
#8758=CARTESIAN_POINT('Origin',(0.,-0.28578,0.));
#8759=CARTESIAN_POINT('Origin',(0.,-0.04763,0.));
#8760=CARTESIAN_POINT('',(0.,0.,0.));
#8761=CARTESIAN_POINT('Origin',(1.013815,0.445,0.));
#8762=CARTESIAN_POINT('',(-1.013815,0.445,-1.24156529467757E-16));
#8763=CARTESIAN_POINT('Origin',(0.,0.445,0.));
#8764=CARTESIAN_POINT('',(-0.991185,0.445,-1.21385153761287E-16));
#8765=CARTESIAN_POINT('Origin',(0.,0.445,0.));
#8766=CARTESIAN_POINT('Origin',(0.,0.4075,0.));
#8767=CARTESIAN_POINT('',(-1.013815,0.37,-1.24156529467757E-16));
#8768=CARTESIAN_POINT('Origin',(0.,0.37,0.));
#8769=CARTESIAN_POINT('',(-1.013815,0.4075,-1.24156529467757E-16));
#8770=CARTESIAN_POINT('Origin',(0.991185,0.37,0.));
#8771=CARTESIAN_POINT('',(-0.991185,0.37,-1.21385153761287E-16));
#8772=CARTESIAN_POINT('Origin',(0.,0.37,0.));
#8773=CARTESIAN_POINT('Origin',(0.,0.4075,0.));
#8774=CARTESIAN_POINT('',(-0.991185,0.4075,-1.21385153761287E-16));
#8775=CARTESIAN_POINT('Origin',(1.013815,-0.37,0.));
#8776=CARTESIAN_POINT('',(-1.013815,-0.37,-1.24156529467757E-16));
#8777=CARTESIAN_POINT('Origin',(0.,-0.37,0.));
#8778=CARTESIAN_POINT('',(-0.991185,-0.37,-1.21385153761287E-16));
#8779=CARTESIAN_POINT('Origin',(0.,-0.37,0.));
#8780=CARTESIAN_POINT('Origin',(0.,-0.4075,0.));
#8781=CARTESIAN_POINT('',(-1.013815,-0.445,-1.24156529467757E-16));
#8782=CARTESIAN_POINT('Origin',(0.,-0.445,0.));
#8783=CARTESIAN_POINT('',(-1.013815,-0.4075,-1.24156529467757E-16));
#8784=CARTESIAN_POINT('Origin',(0.991185,-0.445,0.));
#8785=CARTESIAN_POINT('',(-0.991185,-0.445,-1.21385153761287E-16));
#8786=CARTESIAN_POINT('Origin',(0.,-0.445,0.));
#8787=CARTESIAN_POINT('Origin',(0.,-0.4075,0.));
#8788=CARTESIAN_POINT('',(-0.991185,-0.4075,-1.21385153761287E-16));
#8789=CARTESIAN_POINT('',(0.,0.,0.));
#8790=CARTESIAN_POINT('',(0.,0.,0.));
#8791=CARTESIAN_POINT('',(0.,0.,0.));
#8792=CARTESIAN_POINT('',(0.,0.,0.));
#8793=CARTESIAN_POINT('',(0.,0.,0.));
#8794=CARTESIAN_POINT('',(0.,0.,0.));
#8795=CARTESIAN_POINT('Origin',(0.115470053837925,-0.5,-0.2));
#8796=CARTESIAN_POINT('',(0.23094010767585,-0.5,0.));
#8797=CARTESIAN_POINT('',(0.115470053837925,-0.5,-0.2));
#8798=CARTESIAN_POINT('',(0.23094010767585,-0.5,0.));
#8799=CARTESIAN_POINT('',(0.115470053837925,-0.8,-0.2));
#8800=CARTESIAN_POINT('',(0.115470053837925,-0.5,-0.2));
#8801=CARTESIAN_POINT('',(0.23094010767585,-0.8,0.));
#8802=CARTESIAN_POINT('',(0.23094010767585,-0.8,0.));
#8803=CARTESIAN_POINT('',(0.23094010767585,-0.5,0.));
#8804=CARTESIAN_POINT('Origin',(-0.115470053837925,-0.5,-0.2));
#8805=CARTESIAN_POINT('',(-0.115470053837925,-0.5,-0.2));
#8806=CARTESIAN_POINT('',(0.115470053837925,-0.5,-0.2));
#8807=CARTESIAN_POINT('',(-0.115470053837925,-0.8,-0.2));
#8808=CARTESIAN_POINT('',(-0.115470053837925,-0.5,-0.2));
#8809=CARTESIAN_POINT('',(0.115470053837925,-0.8,-0.2));
#8810=CARTESIAN_POINT('Origin',(-0.23094010767585,-0.5,-2.77555756156289E-17));
#8811=CARTESIAN_POINT('',(-0.23094010767585,-0.5,-2.82820063659975E-17));
#8812=CARTESIAN_POINT('',(-0.115470053837925,-0.5,-0.2));
#8813=CARTESIAN_POINT('',(-0.23094010767585,-0.8,-2.77555756156289E-17));
#8814=CARTESIAN_POINT('',(-0.23094010767585,-0.5,-2.82820063659975E-17));
#8815=CARTESIAN_POINT('',(-0.115470053837925,-0.8,-0.2));
#8816=CARTESIAN_POINT('Origin',(-0.115470053837925,-0.5,0.2));
#8817=CARTESIAN_POINT('',(-0.115470053837925,-0.5,0.2));
#8818=CARTESIAN_POINT('',(-0.23094010767585,-0.5,-2.82820063659975E-17));
#8819=CARTESIAN_POINT('',(-0.115470053837925,-0.8,0.2));
#8820=CARTESIAN_POINT('',(-0.115470053837925,-0.5,0.2));
#8821=CARTESIAN_POINT('',(-0.23094010767585,-0.8,-2.82820063659975E-17));
#8822=CARTESIAN_POINT('Origin',(0.115470053837925,-0.5,0.2));
#8823=CARTESIAN_POINT('',(0.115470053837925,-0.5,0.2));
#8824=CARTESIAN_POINT('',(-0.115470053837925,-0.5,0.2));
#8825=CARTESIAN_POINT('',(0.115470053837925,-0.8,0.2));
#8826=CARTESIAN_POINT('',(0.115470053837925,-0.5,0.2));
#8827=CARTESIAN_POINT('',(-0.115470053837925,-0.8,0.2));
#8828=CARTESIAN_POINT('Origin',(0.23094010767585,-0.5,0.));
#8829=CARTESIAN_POINT('',(0.115470053837925,-0.5,0.2));
#8830=CARTESIAN_POINT('',(0.115470053837925,-0.8,0.2));
#8831=CARTESIAN_POINT('Origin',(0.,-0.5,0.));
#8832=CARTESIAN_POINT('Origin',(0.,-0.8,0.));
#8833=CARTESIAN_POINT('Origin',(0.,-1.4,0.));
#8834=CARTESIAN_POINT('',(-0.24505,-1.4,3.00099698131059E-17));
#8835=CARTESIAN_POINT('Origin',(0.,-1.4,0.));
#8836=CARTESIAN_POINT('Origin',(0.375,0.5,0.));
#8837=CARTESIAN_POINT('',(-0.375,0.5,-4.59242549680257E-17));
#8838=CARTESIAN_POINT('Origin',(0.,0.5,0.));
#8839=CARTESIAN_POINT('Origin',(0.,0.475,0.));
#8840=CARTESIAN_POINT('',(-0.425,0.45,-5.20474889637625E-17));
#8841=CARTESIAN_POINT('Origin',(0.,0.45,0.));
#8842=CARTESIAN_POINT('',(-0.4,0.475,-4.89858719658941E-17));
#8843=CARTESIAN_POINT('Origin',(0.,0.24,0.));
#8844=CARTESIAN_POINT('',(-0.425,0.0299999999999998,-5.20474889637625E-17));
#8845=CARTESIAN_POINT('Origin',(0.,0.0299999999999998,0.));
#8846=CARTESIAN_POINT('',(-0.425,0.24,-5.20474889637625E-17));
#8847=CARTESIAN_POINT('Origin',(0.,0.0150000000000001,0.));
#8848=CARTESIAN_POINT('',(-0.395,4.85722573273506E-17,-4.83735485663204E-17));
#8849=CARTESIAN_POINT('Origin',(0.,0.,0.));
#8850=CARTESIAN_POINT('',(-0.41,0.0150000000000001,-5.02105187650415E-17));
#8851=CARTESIAN_POINT('Origin',(0.27,0.,0.));
#8852=CARTESIAN_POINT('',(-0.27,0.,-3.30654635769785E-17));
#8853=CARTESIAN_POINT('Origin',(0.,0.,0.));
#8854=CARTESIAN_POINT('Origin',(0.,-0.02,0.));
#8855=CARTESIAN_POINT('',(-0.24505,-0.0498999999999999,3.00099698131059E-17));
#8856=CARTESIAN_POINT('Origin',(0.,-0.0498999999999999,0.));
#8857=CARTESIAN_POINT('',(-0.26,-0.02,-3.18408167778312E-17));
#8858=CARTESIAN_POINT('Origin',(0.,-0.995,0.));
#8859=CARTESIAN_POINT('',(-0.24505,-0.995,-3.00099698131059E-17));
#8860=CARTESIAN_POINT('',(0.,0.,0.));
#8861=CARTESIAN_POINT('Origin',(0.0866025403784439,-0.4,-0.15));
#8862=CARTESIAN_POINT('',(0.173205080756888,-0.4,0.));
#8863=CARTESIAN_POINT('',(0.0866025403784439,-0.4,-0.15));
#8864=CARTESIAN_POINT('',(0.173205080756888,-0.4,0.));
#8865=CARTESIAN_POINT('',(0.0866025403784439,-0.64,-0.15));
#8866=CARTESIAN_POINT('',(0.0866025403784439,-0.4,-0.15));
#8867=CARTESIAN_POINT('',(0.173205080756888,-0.64,0.));
#8868=CARTESIAN_POINT('',(0.173205080756888,-0.64,0.));
#8869=CARTESIAN_POINT('',(0.173205080756888,-0.4,0.));
#8870=CARTESIAN_POINT('Origin',(-0.0866025403784438,-0.4,-0.15));
#8871=CARTESIAN_POINT('',(-0.0866025403784438,-0.4,-0.15));
#8872=CARTESIAN_POINT('',(0.0866025403784439,-0.4,-0.15));
#8873=CARTESIAN_POINT('',(-0.0866025403784438,-0.64,-0.15));
#8874=CARTESIAN_POINT('',(-0.0866025403784438,-0.4,-0.15));
#8875=CARTESIAN_POINT('',(0.0866025403784439,-0.64,-0.15));
#8876=CARTESIAN_POINT('Origin',(-0.173205080756888,-0.4,-2.77555756156289E-17));
#8877=CARTESIAN_POINT('',(-0.173205080756888,-0.4,-2.12115047744981E-17));
#8878=CARTESIAN_POINT('',(-0.0866025403784438,-0.4,-0.15));
#8879=CARTESIAN_POINT('',(-0.173205080756888,-0.64,-2.77555756156289E-17));
#8880=CARTESIAN_POINT('',(-0.173205080756888,-0.4,-2.12115047744981E-17));
#8881=CARTESIAN_POINT('',(-0.0866025403784438,-0.64,-0.15));
#8882=CARTESIAN_POINT('Origin',(-0.0866025403784439,-0.4,0.15));
#8883=CARTESIAN_POINT('',(-0.0866025403784439,-0.4,0.15));
#8884=CARTESIAN_POINT('',(-0.173205080756888,-0.4,-2.12115047744981E-17));
#8885=CARTESIAN_POINT('',(-0.0866025403784439,-0.64,0.15));
#8886=CARTESIAN_POINT('',(-0.0866025403784439,-0.4,0.15));
#8887=CARTESIAN_POINT('',(-0.173205080756888,-0.64,-2.12115047744981E-17));
#8888=CARTESIAN_POINT('Origin',(0.0866025403784439,-0.4,0.15));
#8889=CARTESIAN_POINT('',(0.0866025403784439,-0.4,0.15));
#8890=CARTESIAN_POINT('',(-0.0866025403784439,-0.4,0.15));
#8891=CARTESIAN_POINT('',(0.0866025403784439,-0.64,0.15));
#8892=CARTESIAN_POINT('',(0.0866025403784439,-0.4,0.15));
#8893=CARTESIAN_POINT('',(-0.0866025403784439,-0.64,0.15));
#8894=CARTESIAN_POINT('Origin',(0.173205080756888,-0.4,0.));
#8895=CARTESIAN_POINT('',(0.0866025403784439,-0.4,0.15));
#8896=CARTESIAN_POINT('',(0.0866025403784439,-0.64,0.15));
#8897=CARTESIAN_POINT('Origin',(0.,-0.4,-2.77555756156289E-17));
#8898=CARTESIAN_POINT('Origin',(0.,-0.64,-2.77555756156289E-17));
#8899=CARTESIAN_POINT('Origin',(0.,-1.,0.));
#8900=CARTESIAN_POINT('',(-0.1954,-1.,2.39295984553393E-17));
#8901=CARTESIAN_POINT('Origin',(0.,-1.,0.));
#8902=CARTESIAN_POINT('Origin',(0.3,0.4,0.));
#8903=CARTESIAN_POINT('',(-0.3,0.4,-3.67394039744206E-17));
#8904=CARTESIAN_POINT('Origin',(0.,0.4,0.));
#8905=CARTESIAN_POINT('Origin',(0.,0.375,0.));
#8906=CARTESIAN_POINT('',(-0.35,0.35,-4.28626379701573E-17));
#8907=CARTESIAN_POINT('Origin',(0.,0.35,0.));
#8908=CARTESIAN_POINT('',(-0.325,0.375,-3.9801020972289E-17));
#8909=CARTESIAN_POINT('Origin',(0.,0.19,0.));
#8910=CARTESIAN_POINT('',(-0.35,0.03,-4.28626379701574E-17));
#8911=CARTESIAN_POINT('Origin',(0.,0.03,0.));
#8912=CARTESIAN_POINT('',(-0.35,0.19,-4.28626379701574E-17));
#8913=CARTESIAN_POINT('Origin',(0.,0.0149999999999999,0.));
#8914=CARTESIAN_POINT('',(-0.32,-3.29597460435593E-17,-3.91886975727153E-17));
#8915=CARTESIAN_POINT('Origin',(0.,0.,0.));
#8916=CARTESIAN_POINT('',(-0.335,0.0149999999999999,-4.10256677714363E-17));
#8917=CARTESIAN_POINT('Origin',(0.22,0.,0.));
#8918=CARTESIAN_POINT('',(-0.22,-6.93889390390723E-18,-2.69422295812418E-17));
#8919=CARTESIAN_POINT('Origin',(0.,0.,0.));
#8920=CARTESIAN_POINT('Origin',(0.,-0.02,0.));
#8921=CARTESIAN_POINT('',(-0.1954,-0.0492,2.39295984553393E-17));
#8922=CARTESIAN_POINT('Origin',(0.,-0.0492,0.));
#8923=CARTESIAN_POINT('',(-0.21,-0.02,-2.57175827820944E-17));
#8924=CARTESIAN_POINT('Origin',(0.,-0.8,0.));
#8925=CARTESIAN_POINT('',(-0.1954,-0.8,-2.39295984553393E-17));
#8926=CARTESIAN_POINT('',(0.,0.,0.));
#8927=CARTESIAN_POINT('Ctrl Pts',(0.662463988280159,-0.0499822726657336,
-2.00015029073282));
#8928=CARTESIAN_POINT('Ctrl Pts',(0.662719098649113,-0.050156409826639,
-1.8362081654112));
#8929=CARTESIAN_POINT('Ctrl Pts',(0.661897332210143,-0.0496009500256405,
-1.51421284590545));
#8930=CARTESIAN_POINT('Ctrl Pts',(0.662849183916153,-0.050231417425612,
-1.10458538375921));
#8931=CARTESIAN_POINT('Ctrl Pts',(0.662676266642772,-0.050132523365314,
-0.778488486630415));
#8932=CARTESIAN_POINT('Ctrl Pts',(0.660820022877162,-0.0488315955858374,
-0.544415125004604));
#8933=CARTESIAN_POINT('Ctrl Pts',(0.663563470597623,-0.0508446374556383,
-0.288026483088336));
#8934=CARTESIAN_POINT('Ctrl Pts',(0.667640080240138,-0.0524139639419364,
-0.0320317672708526));
#8935=CARTESIAN_POINT('Ctrl Pts',(0.65335380658105,-0.0455068140358546,
0.139218056313768));
#8936=CARTESIAN_POINT('Ctrl Pts',(0.611163697009464,-0.0383525034286994,
0.264648815779984));
#8937=CARTESIAN_POINT('Ctrl Pts',(0.548065973192159,-0.032280894159065,
0.384307758714896));
#8938=CARTESIAN_POINT('Ctrl Pts',(0.431002395435098,-0.0256993836631372,
0.520971575878654));
#8939=CARTESIAN_POINT('Ctrl Pts',(0.191480329024041,-0.0134075415523006,
0.662765347245377));
#8940=CARTESIAN_POINT('Ctrl Pts',(-0.170310845287768,0.00096264921625724,
0.690490277729099));
#8941=CARTESIAN_POINT('Ctrl Pts',(-0.585085784735021,0.0207569079373872,
0.435755076168825));
#8942=CARTESIAN_POINT('Ctrl Pts',(-0.744693743478759,0.0422927786570434,
-0.0951523515529584));
#8943=CARTESIAN_POINT('Ctrl Pts',(-0.431538112822807,0.0659892634348224,
-0.617104732797172));
#8944=CARTESIAN_POINT('Ctrl Pts',(0.115758946274973,0.0876905285771165,
-0.725599039992233));
#8945=CARTESIAN_POINT('Ctrl Pts',(0.53747991286649,0.107478289621193,-0.475188997283933));
#8946=CARTESIAN_POINT('Ctrl Pts',(0.715006044039375,0.125301300434412,-0.0720347673296787));
#8947=CARTESIAN_POINT('Ctrl Pts',(0.622824528841228,0.143151007884386,0.360207879087552));
#8948=CARTESIAN_POINT('Ctrl Pts',(0.295215046776041,0.161020056779893,0.657018975821946));
#8949=CARTESIAN_POINT('Ctrl Pts',(-0.144725676703892,0.178909769816401,
0.70633098622582));
#8950=CARTESIAN_POINT('Ctrl Pts',(-0.530690929834931,0.196817259725453,
0.489300976461692));
#8951=CARTESIAN_POINT('Ctrl Pts',(-0.717478987054585,0.214742051156983,
0.086194632105411));
#8952=CARTESIAN_POINT('Ctrl Pts',(-0.641992299862074,0.230688881084643,
-0.299876917809462));
#8953=CARTESIAN_POINT('Ctrl Pts',(-0.36030002070441,0.248640851668397,-0.629569645495563));
#8954=CARTESIAN_POINT('Ctrl Pts',(0.0867941523773002,0.266605918529927,
-0.737064913155744));
#8955=CARTESIAN_POINT('Ctrl Pts',(0.522621279421028,0.286581789189134,-0.500819963452499));
#8956=CARTESIAN_POINT('Ctrl Pts',(0.740365136709862,0.306568406437996,-0.0577085025886233));
#8957=CARTESIAN_POINT('Ctrl Pts',(0.588086029972563,0.328565375698038,0.488053495238463));
#8958=CARTESIAN_POINT('Ctrl Pts',(0.0972167907293641,0.34990603829391,0.730574719890591));
#8959=CARTESIAN_POINT('Ctrl Pts',(-0.348606790473969,0.368583951861805,
0.625079898555237));
#8960=CARTESIAN_POINT('Ctrl Pts',(-0.625117601034868,0.384596133557627,
0.348183842295094));
#8961=CARTESIAN_POINT('Ctrl Pts',(-0.731235197502955,0.403278517609434,
-0.0977683708505558));
#8962=CARTESIAN_POINT('Ctrl Pts',(-0.487350453008389,0.424630334656425,
-0.588208599365547));
#8963=CARTESIAN_POINT('Ctrl Pts',(0.107586035230619,0.448648433132338,-0.756188390862319));
#8964=CARTESIAN_POINT('Ctrl Pts',(0.630965640778732,0.472660315479601,-0.429375166251397));
#8965=CARTESIAN_POINT('Ctrl Pts',(0.742175157663465,0.496662180030771,0.177201798791322));
#8966=CARTESIAN_POINT('Ctrl Pts',(0.367484330759339,0.520650735211898,0.667598289986901));
#8967=CARTESIAN_POINT('Ctrl Pts',(-0.1772094561828,0.541959207305282,0.714834645121414));
#8968=CARTESIAN_POINT('Ctrl Pts',(-0.55158365946692,0.56059094898577,0.452401551542145));
#8969=CARTESIAN_POINT('Ctrl Pts',(-0.707144881750632,0.57655098007586,0.0945309854926571));
#8970=CARTESIAN_POINT('Ctrl Pts',(-0.650080156703408,0.592499998475874,
-0.292288521076879));
#8971=CARTESIAN_POINT('Ctrl Pts',(-0.39813025511233,0.608437064253082,-0.590670145737896));
#8972=CARTESIAN_POINT('Ctrl Pts',(-0.0275908863199736,0.62436100859898,
-0.710669286038228));
#8973=CARTESIAN_POINT('Ctrl Pts',(0.414715655942592,0.642922729480766,-0.603621999120373));
#8974=CARTESIAN_POINT('Ctrl Pts',(0.73835387107679,0.664111160627632,-0.166965130048199));
#8975=CARTESIAN_POINT('Ctrl Pts',(0.620304111002753,0.687911568470837,0.433769461113443));
#8976=CARTESIAN_POINT('Ctrl Pts',(0.0958337440893244,0.711671376372341,
0.74830999711301));
#8977=CARTESIAN_POINT('Ctrl Pts',(-0.328971586153759,0.728968689390915,
0.621190836988033));
#8978=CARTESIAN_POINT('Ctrl Pts',(-0.510250580429896,0.739824441432273,
0.439145396424497));
#8979=CARTESIAN_POINT('Ctrl Pts',(-0.592478248153049,0.74570751472679,0.326342499792088));
#8980=CARTESIAN_POINT('Ctrl Pts',(-0.689058767063034,0.756222082569521,
0.0984146554749596));
#8981=CARTESIAN_POINT('Ctrl Pts',(-0.666219044663549,0.767653433960867,
-0.192704218915611));
#8982=CARTESIAN_POINT('Ctrl Pts',(-0.523816993927788,0.780063785948551,
-0.433645748061385));
#8983=CARTESIAN_POINT('Ctrl Pts',(-0.386340473147736,0.786669200591926,
-0.551372175845378));
#8984=CARTESIAN_POINT('Ctrl Pts',(-0.265956682682317,0.792781771671027,
-0.614881276898037));
#8985=CARTESIAN_POINT('Ctrl Pts',(-0.139596638836966,0.799988366367406,
-0.657366153595634));
#8986=CARTESIAN_POINT('Ctrl Pts',(0.0321180206196141,0.806907294366097,
-0.671653874643804));
#8987=CARTESIAN_POINT('Ctrl Pts',(0.288027302850487,0.805335668320584,-0.667586118918959));
#8988=CARTESIAN_POINT('Ctrl Pts',(0.54442707625171,0.8033242699894,-0.664844003722482));
#8989=CARTESIAN_POINT('Ctrl Pts',(0.778488091977107,0.804624888614752,-0.666703265676913));
#8990=CARTESIAN_POINT('Ctrl Pts',(1.10459263968738,0.804724235202262,-0.66687751216757));
#8991=CARTESIAN_POINT('Ctrl Pts',(1.51421119194035,0.804093904068503,-0.665928948647562));
#8992=CARTESIAN_POINT('Ctrl Pts',(1.83620821687538,0.804649660698633,-0.66675251787415));
#8993=CARTESIAN_POINT('Ctrl Pts',(2.00015071794412,0.804475523135573,-0.666497406911305));
#8994=CARTESIAN_POINT('Ctrl Pts',(0.674446082047605,-0.0350079680470159,
-2.0001530305623));
#8995=CARTESIAN_POINT('Ctrl Pts',(0.674701196382384,-0.0351821079149749,
-1.83620835667417));
#8996=CARTESIAN_POINT('Ctrl Pts',(0.673880936475708,-0.0346263233539259,
-1.51419872926041));
#8997=CARTESIAN_POINT('Ctrl Pts',(0.674833527244618,-0.0352575894449097,
-1.10460499764898));
#8998=CARTESIAN_POINT('Ctrl Pts',(0.674662892741623,-0.0351576445284815,
-0.778466545112985));
#8999=CARTESIAN_POINT('Ctrl Pts',(0.67280508837135,-0.0338589215885485,
-0.544434301215379));
#9000=CARTESIAN_POINT('Ctrl Pts',(0.675556714498639,-0.0358668037102216,
-0.288024615576321));
#9001=CARTESIAN_POINT('Ctrl Pts',(0.679620952141269,-0.0374476933188151,
-0.032249939480985));
#9002=CARTESIAN_POINT('Ctrl Pts',(0.665348834630966,-0.0305040167873278,
0.14048082279948));
#9003=CARTESIAN_POINT('Ctrl Pts',(0.62228669882739,-0.0231938376451895,
0.268666180783973));
#9004=CARTESIAN_POINT('Ctrl Pts',(0.557982182284105,-0.0170103722728659,
0.390533052942412));
#9005=CARTESIAN_POINT('Ctrl Pts',(0.438991286666523,-0.0103201349719665,
0.52946260531362));
#9006=CARTESIAN_POINT('Ctrl Pts',(0.195264943047363,0.00218717191725961,
0.673765355231291));
#9007=CARTESIAN_POINT('Ctrl Pts',(-0.172425934555583,0.0167901354760882,
0.701847369499063));
#9008=CARTESIAN_POINT('Ctrl Pts',(-0.593820028218252,0.0369011555335372,
0.443051917288691));
#9009=CARTESIAN_POINT('Ctrl Pts',(-0.755714874644402,0.0587598776212364,
-0.0959321206050264));
#9010=CARTESIAN_POINT('Ctrl Pts',(-0.43801433194566,0.0827940205198624,
-0.625251628852071));
#9011=CARTESIAN_POINT('Ctrl Pts',(0.116602046289419,0.104783098701226,-0.735092792907372));
#9012=CARTESIAN_POINT('Ctrl Pts',(0.543561315738589,0.124817673728603,-0.481501423919919));
#9013=CARTESIAN_POINT('Ctrl Pts',(0.723146404942936,0.142850573437901,-0.073564714561987));
#9014=CARTESIAN_POINT('Ctrl Pts',(0.629891273516298,0.160897879216403,0.363473014402678));
#9015=CARTESIAN_POINT('Ctrl Pts',(0.298840430266652,0.178952078689978,0.663337021281643));
#9016=CARTESIAN_POINT('Ctrl Pts',(-0.145370129699683,0.19701439207729,0.713079165107859));
#9017=CARTESIAN_POINT('Ctrl Pts',(-0.534777464258203,0.215081700570601,
0.494059450643713));
#9018=CARTESIAN_POINT('Ctrl Pts',(-0.723059497631479,0.233153598058585,
0.087604707943711));
#9019=CARTESIAN_POINT('Ctrl Pts',(-0.646967875903001,0.249219385062332,
-0.301358039243341));
#9020=CARTESIAN_POINT('Ctrl Pts',(-0.363297994601133,0.26729513369037,-0.633323883813959));
#9021=CARTESIAN_POINT('Ctrl Pts',(0.0865905388130023,0.285371192232844,
-0.741400774225685));
#9022=CARTESIAN_POINT('Ctrl Pts',(0.524706169760779,0.305452127192914,-0.503845943167671));
#9023=CARTESIAN_POINT('Ctrl Pts',(0.743402185160331,0.325530022126121,-0.058664817656703));
#9024=CARTESIAN_POINT('Ctrl Pts',(0.590448745665821,0.347606360017064,0.48909521564047));
#9025=CARTESIAN_POINT('Ctrl Pts',(0.0981851250008973,0.369004878005666,
0.732177168636611));
#9026=CARTESIAN_POINT('Ctrl Pts',(-0.348488468098564,0.387718276399827,
0.626441749101411));
#9027=CARTESIAN_POINT('Ctrl Pts',(-0.62532356257491,0.403750121631928,0.34916763101975));
#9028=CARTESIAN_POINT('Ctrl Pts',(-0.73146453597972,0.422443135444508,-0.0970695459087969));
#9029=CARTESIAN_POINT('Ctrl Pts',(-0.487535521710562,0.443787780507866,
-0.587339074779301));
#9030=CARTESIAN_POINT('Ctrl Pts',(0.106710568101606,0.467775062885446,-0.75498659819416));
#9031=CARTESIAN_POINT('Ctrl Pts',(0.628862026286412,0.49173208797649,-0.428789598129798));
#9032=CARTESIAN_POINT('Ctrl Pts',(0.739595803505217,0.515655142144853,0.175870704718188));
#9033=CARTESIAN_POINT('Ctrl Pts',(0.366376505463985,0.539541361351028,0.664120189316023));
#9034=CARTESIAN_POINT('Ctrl Pts',(-0.175506327148597,0.560738153809924,
0.711020492425908));
#9035=CARTESIAN_POINT('Ctrl Pts',(-0.54760485001816,0.579257515342459,0.450116428906716));
#9036=CARTESIAN_POINT('Ctrl Pts',(-0.702114990885751,0.595111390068342,
0.0946054547014213));
#9037=CARTESIAN_POINT('Ctrl Pts',(-0.645425496799589,0.610942449002933,
-0.289378750952378));
#9038=CARTESIAN_POINT('Ctrl Pts',(-0.395457432624221,0.626751558207065,
-0.585362642366029));
#9039=CARTESIAN_POINT('Ctrl Pts',(-0.0280797855644617,0.642538439860898,
-0.704297505820287));
#9040=CARTESIAN_POINT('Ctrl Pts',(0.410157779824956,0.660929008716659,-0.598194594147799));
#9041=CARTESIAN_POINT('Ctrl Pts',(0.730444289398745,0.681901601594788,-0.165864021920736));
#9042=CARTESIAN_POINT('Ctrl Pts',(0.613580247437332,0.705441153426337,0.428286178430747));
#9043=CARTESIAN_POINT('Ctrl Pts',(0.0952918314245258,0.72891509356906,0.738958605866823));
#9044=CARTESIAN_POINT('Ctrl Pts',(-0.324020729601473,0.745988444923654,
0.613400639649111));
#9045=CARTESIAN_POINT('Ctrl Pts',(-0.502873233709575,0.756698580939822,
0.433790954112853));
#9046=CARTESIAN_POINT('Ctrl Pts',(-0.583995235083359,0.762502876341029,
0.322496949785477));
#9047=CARTESIAN_POINT('Ctrl Pts',(-0.67925606222965,0.772870829077922,0.0977335101944516));
#9048=CARTESIAN_POINT('Ctrl Pts',(-0.65666377058204,0.784140125347959,-0.189261322798156));
#9049=CARTESIAN_POINT('Ctrl Pts',(-0.516444187283226,0.796361392235239,
-0.426530997573169));
#9050=CARTESIAN_POINT('Ctrl Pts',(-0.380942240338964,0.802871714443619,
-0.542569702523433));
#9051=CARTESIAN_POINT('Ctrl Pts',(-0.262525555833722,0.808884384740767,
-0.604997953335358));
#9052=CARTESIAN_POINT('Ctrl Pts',(-0.138595359825784,0.81595371167701,-0.646716670398854));
#9053=CARTESIAN_POINT('Ctrl Pts',(0.0319355517137274,0.822844653227088,
-0.661020222212807));
#9054=CARTESIAN_POINT('Ctrl Pts',(0.288093504695908,0.821281075632325,-0.656931006487794));
#9055=CARTESIAN_POINT('Ctrl Pts',(0.544427040001579,0.819265409799516,-0.654193021724466));
#9056=CARTESIAN_POINT('Ctrl Pts',(0.778506679323761,0.820567398055238,-0.65604695266566));
#9057=CARTESIAN_POINT('Ctrl Pts',(1.10459883628042,0.820665745979243,-0.656221018219063));
#9058=CARTESIAN_POINT('Ctrl Pts',(1.51421765241308,0.820035614746722,-0.6552683862334));
#9059=CARTESIAN_POINT('Ctrl Pts',(1.83620811434072,0.820590881682782,-0.656090536299704));
#9060=CARTESIAN_POINT('Ctrl Pts',(2.00015105938536,0.820416743648137,-0.655835424645988));
#9061=CARTESIAN_POINT('Ctrl Pts',(0.687145391337529,0.00388813180289089,
-2.00013147703594));
#9062=CARTESIAN_POINT('Ctrl Pts',(0.687400475859769,0.0037140122848332,
-1.83620596164366));
#9063=CARTESIAN_POINT('Ctrl Pts',(0.686580688274375,0.00426996159012147,
-1.51426120920445));
#9064=CARTESIAN_POINT('Ctrl Pts',(0.687528287675259,0.00363896296830716,
-1.10450912461653));
#9065=CARTESIAN_POINT('Ctrl Pts',(0.687361410679772,0.00373905286893215,
-0.778550764556369));
#9066=CARTESIAN_POINT('Ctrl Pts',(0.685492998268397,0.00503776682278646,
-0.544450526600379));
#9067=CARTESIAN_POINT('Ctrl Pts',(0.688265132824333,0.00303048983174741,
-0.287682055551203));
#9068=CARTESIAN_POINT('Ctrl Pts',(0.692275545237537,0.00144918010494716,
-0.0326506971997516));
#9069=CARTESIAN_POINT('Ctrl Pts',(0.67811721874054,0.00839277279208392,
0.140578602255062));
#9070=CARTESIAN_POINT('Ctrl Pts',(0.63417051039127,0.0158657021192725,0.271702248096095));
#9071=CARTESIAN_POINT('Ctrl Pts',(0.568467937345546,0.0221776380697667,
0.396075371092485));
#9072=CARTESIAN_POINT('Ctrl Pts',(0.447630344944513,0.0289704247052655,
0.537162845625327));
#9073=CARTESIAN_POINT('Ctrl Pts',(0.199876057358082,0.0416847890516129,
0.683850399068708));
#9074=CARTESIAN_POINT('Ctrl Pts',(-0.173340277410583,0.0565066590856592,
0.712241041234605));
#9075=CARTESIAN_POINT('Ctrl Pts',(-0.600363534440907,0.0768907360741932,
0.449858568469966));
#9076=CARTESIAN_POINT('Ctrl Pts',(-0.763917267702635,0.0990052380588372,
-0.0954913299225577));
#9077=CARTESIAN_POINT('Ctrl Pts',(-0.442946718272606,0.123269337596085,
-0.629705813071489));
#9078=CARTESIAN_POINT('Ctrl Pts',(0.115829754215989,0.14542261482116,-0.740117721914303));
#9079=CARTESIAN_POINT('Ctrl Pts',(0.545089263156225,0.16557013801192,-0.485003463987623));
#9080=CARTESIAN_POINT('Ctrl Pts',(0.725288867731711,0.183675686835684,-0.0754012297787415));
#9081=CARTESIAN_POINT('Ctrl Pts',(0.631698822495185,0.201767226924317,0.362657949057064));
#9082=CARTESIAN_POINT('Ctrl Pts',(0.300308325987629,0.219836949162313,0.662675815052713));
#9083=CARTESIAN_POINT('Ctrl Pts',(-0.143562158262448,0.237886151027376,
0.712267282797029));
#9084=CARTESIAN_POINT('Ctrl Pts',(-0.53199081656655,0.255911794003117,0.493667448281364));
#9085=CARTESIAN_POINT('Ctrl Pts',(-0.719417883604853,0.273913307071238,
0.0887760590256471));
#9086=CARTESIAN_POINT('Ctrl Pts',(-0.643660400053528,0.289891600721182,
-0.298017275867573));
#9087=CARTESIAN_POINT('Ctrl Pts',(-0.361885010363615,0.30784406213564,-0.627666996846731));
#9088=CARTESIAN_POINT('Ctrl Pts',(0.0842417800773362,0.325768011230139,
-0.734653870518568));
#9089=CARTESIAN_POINT('Ctrl Pts',(0.517792745159868,0.345644945040527,-0.499418060334344));
#9090=CARTESIAN_POINT('Ctrl Pts',(0.733800619596213,0.365486255885401,-0.0594459732028802));
#9091=CARTESIAN_POINT('Ctrl Pts',(0.582673221392261,0.387265364391542,0.480796666749224));
#9092=CARTESIAN_POINT('Ctrl Pts',(0.0980556067817179,0.408328917576356,
0.719856122275624));
#9093=CARTESIAN_POINT('Ctrl Pts',(-0.340801028355373,0.426717108826706,
0.615863970111398));
#9094=CARTESIAN_POINT('Ctrl Pts',(-0.612394281678541,0.442448812919543,
0.343756687773024));
#9095=CARTESIAN_POINT('Ctrl Pts',(-0.716305141601163,0.460766578913181,
-0.0935336978388081));
#9096=CARTESIAN_POINT('Ctrl Pts',(-0.477493247204526,0.481649255554787,
-0.573041994394618));
#9097=CARTESIAN_POINT('Ctrl Pts',(0.102694969855398,0.505068049619363,-0.736450132310173));
#9098=CARTESIAN_POINT('Ctrl Pts',(0.611261259282936,0.528410394709111,-0.418440438696257));
#9099=CARTESIAN_POINT('Ctrl Pts',(0.718676149949771,0.551673390367526,0.169515917432784));
#9100=CARTESIAN_POINT('Ctrl Pts',(0.356312681653224,0.574854495176515,0.64316080321234));
#9101=CARTESIAN_POINT('Ctrl Pts',(-0.168510516307296,0.595385048110979,
0.688354852013418));
#9102=CARTESIAN_POINT('Ctrl Pts',(-0.528243301677406,0.613292864691495,
0.436029414275985));
#9103=CARTESIAN_POINT('Ctrl Pts',(-0.677381584882317,0.6286030155416,0.0926943249944734));
#9104=CARTESIAN_POINT('Ctrl Pts',(-0.622643305904953,0.643873929815472,
-0.277654803412519));
#9105=CARTESIAN_POINT('Ctrl Pts',(-0.381794378299548,0.65910436568187,-0.562730607759754));
#9106=CARTESIAN_POINT('Ctrl Pts',(-0.028341775812421,0.674293171253774,
-0.677102900368987));
#9107=CARTESIAN_POINT('Ctrl Pts',(0.392731635988073,0.691964896901324,-0.575070914546373));
#9108=CARTESIAN_POINT('Ctrl Pts',(0.69992938794118,0.712091816947967,-0.160128547586193));
#9109=CARTESIAN_POINT('Ctrl Pts',(0.587760439579667,0.734637493639678,0.408855815692916));
#9110=CARTESIAN_POINT('Ctrl Pts',(0.0921415777392107,0.757083566082351,
0.705744227349691));
#9111=CARTESIAN_POINT('Ctrl Pts',(-0.308102004413837,0.773385243522869,
0.585710561547649));
#9112=CARTESIAN_POINT('Ctrl Pts',(-0.478599554075341,0.783594714378652,
0.414507861658026));
#9113=CARTESIAN_POINT('Ctrl Pts',(-0.555934555524573,0.789130340065261,
0.308363588185029));
#9114=CARTESIAN_POINT('Ctrl Pts',(-0.646753984994522,0.799002819487883,
0.0943350303702933));
#9115=CARTESIAN_POINT('Ctrl Pts',(-0.62495936464493,0.809749811628134,-0.179246402023147));
#9116=CARTESIAN_POINT('Ctrl Pts',(-0.491908913808404,0.821352972100955,
-0.404491410613556));
#9117=CARTESIAN_POINT('Ctrl Pts',(-0.362868577423681,0.827552900541956,
-0.515047589824164));
#9118=CARTESIAN_POINT('Ctrl Pts',(-0.250447563309727,0.833262939476477,
-0.574215859282791));
#9119=CARTESIAN_POINT('Ctrl Pts',(-0.134136950448111,0.839898037093364,
-0.613487677738248));
#9120=CARTESIAN_POINT('Ctrl Pts',(0.0314794347668697,0.846658718841028,
-0.627750772072444));
#9121=CARTESIAN_POINT('Ctrl Pts',(0.287859120913106,0.845135120072913,-0.623654695722356));
#9122=CARTESIAN_POINT('Ctrl Pts',(0.544382169584791,0.843101510843351,-0.620927805523985));
#9123=CARTESIAN_POINT('Ctrl Pts',(0.778656772185477,0.844411082457674,-0.62278249525087));
#9124=CARTESIAN_POINT('Ctrl Pts',(1.1044633350947,0.844505710507847,-0.622960502431314));
#9125=CARTESIAN_POINT('Ctrl Pts',(1.51431720637969,0.843878360419051,-0.622011929608527));
#9126=CARTESIAN_POINT('Ctrl Pts',(1.83620514057881,0.844432460340288,-0.622837578949083));
#9127=CARTESIAN_POINT('Ctrl Pts',(2.00012463874466,0.844258347210608,-0.62258250378106));
#9128=CARTESIAN_POINT('Ctrl Pts',(0.665690148929301,0.0540139888223781,
-2.00004484750611));
#9129=CARTESIAN_POINT('Ctrl Pts',(0.6659451150026,0.053839950157021,-1.83619545121158));
#9130=CARTESIAN_POINT('Ctrl Pts',(0.665128143222169,0.0543938477409031,
-1.51455427814217));
#9131=CARTESIAN_POINT('Ctrl Pts',(0.666069495045158,0.0537665346002613,
-1.10412981632951));
#9132=CARTESIAN_POINT('Ctrl Pts',(0.665911310936667,0.0538607932718387,
-0.778993035250902));
#9133=CARTESIAN_POINT('Ctrl Pts',(0.664026136107024,0.0551700417313962,
-0.544470742495059));
#9134=CARTESIAN_POINT('Ctrl Pts',(0.666838914554533,0.0531361927202069,
-0.286662280700477));
#9135=CARTESIAN_POINT('Ctrl Pts',(0.670756199727559,0.0516121409687555,
-0.0329492975889785));
#9136=CARTESIAN_POINT('Ctrl Pts',(0.656928056566985,0.0583614640101509,
0.134122099891118));
#9137=CARTESIAN_POINT('Ctrl Pts',(0.614653651087194,0.0655518749768497,
0.260460791549869));
#9138=CARTESIAN_POINT('Ctrl Pts',(0.550691302932979,0.0716990222856046,
0.381491744797825));
#9139=CARTESIAN_POINT('Ctrl Pts',(0.433937868706107,0.0782551569430249,
0.517766096947181));
#9140=CARTESIAN_POINT('Ctrl Pts',(0.195022227157333,0.0905176840738019,
0.659128805501105));
#9141=CARTESIAN_POINT('Ctrl Pts',(-0.165221803132377,0.104824365687565,
0.686656794439709));
#9142=CARTESIAN_POINT('Ctrl Pts',(-0.575948987297183,0.124434718794426,
0.433851544302891));
#9143=CARTESIAN_POINT('Ctrl Pts',(-0.73284398024972,0.145673674627877,-0.0898275556952109));
#9144=CARTESIAN_POINT('Ctrl Pts',(-0.425082855843943,0.168912723107633,
-0.601402499618176));
#9145=CARTESIAN_POINT('Ctrl Pts',(0.108828702060105,0.19007897377441,-0.706601840568686));
#9146=CARTESIAN_POINT('Ctrl Pts',(0.517997291942158,0.209286498552809,-0.463265327584241));
#9147=CARTESIAN_POINT('Ctrl Pts',(0.689377950201828,0.226516243592352,-0.0734161361504486));
#9148=CARTESIAN_POINT('Ctrl Pts',(0.600353887084564,0.243701687466735,0.342693377829791));
#9149=CARTESIAN_POINT('Ctrl Pts',(0.286030035028936,0.260835983707096,0.627102830068772));
#9150=CARTESIAN_POINT('Ctrl Pts',(-0.134155065157305,0.277920950638178,
0.673933998676897));
#9151=CARTESIAN_POINT('Ctrl Pts',(-0.501164021709181,0.294954365139144,
0.467262210920895));
#9152=CARTESIAN_POINT('Ctrl Pts',(-0.677874728226525,0.311936243936039,
0.0852452309648463));
#9153=CARTESIAN_POINT('Ctrl Pts',(-0.606442919414857,0.326984295200526,
-0.279024712472493));
#9154=CARTESIAN_POINT('Ctrl Pts',(-0.3413638889742,0.343869213947561,-0.589050402985317));
#9155=CARTESIAN_POINT('Ctrl Pts',(0.0776127328996499,0.360700417795057,
-0.689346797344412));
#9156=CARTESIAN_POINT('Ctrl Pts',(0.483925382117204,0.379330610399405,-0.468750804288638));
#9157=CARTESIAN_POINT('Ctrl Pts',(0.685993707862927,0.397899656052825,-0.0569247093507329));
#9158=CARTESIAN_POINT('Ctrl Pts',(0.544593843892337,0.41824532301881,0.447745369014097));
#9159=CARTESIAN_POINT('Ctrl Pts',(0.0926262835585758,0.437885829762225,
0.670478864626929));
#9160=CARTESIAN_POINT('Ctrl Pts',(-0.315940435227643,0.455005455676549,
0.573590148682299));
#9161=CARTESIAN_POINT('Ctrl Pts',(-0.56845556554157,0.469633957922228,0.320516289738299));
#9162=CARTESIAN_POINT('Ctrl Pts',(-0.664899902133018,0.486647192977617,
-0.0856672750405439));
#9163=CARTESIAN_POINT('Ctrl Pts',(-0.443255626672905,0.506013771825995,
-0.530317040586));
#9164=CARTESIAN_POINT('Ctrl Pts',(0.0940211962866315,0.527697344618731,
-0.681439042050755));
#9165=CARTESIAN_POINT('Ctrl Pts',(0.564092381788613,0.549276072844908,-0.387291286681534));
#9166=CARTESIAN_POINT('Ctrl Pts',(0.663088983781026,0.570749464526914,0.155497762155742));
#9167=CARTESIAN_POINT('Ctrl Pts',(0.328929597234121,0.592117299617171,0.592008544234696));
#9168=CARTESIAN_POINT('Ctrl Pts',(-0.154237322206182,0.611016959266645,
0.633500441753773));
#9169=CARTESIAN_POINT('Ctrl Pts',(-0.485035884449274,0.627485653531596,
0.401403084621955));
#9170=CARTESIAN_POINT('Ctrl Pts',(-0.62206334875908,0.641554792618914,0.0858794376383043));
#9171=CARTESIAN_POINT('Ctrl Pts',(-0.571760075942313,0.655576455451205,
-0.254188255862264));
#9172=CARTESIAN_POINT('Ctrl Pts',(-0.350733148500619,0.669551327422222,
-0.51575472245803));
#9173=CARTESIAN_POINT('Ctrl Pts',(-0.0265957997704319,0.683479439931836,
-0.620606617386987));
#9174=CARTESIAN_POINT('Ctrl Pts',(0.35930180280925,0.699674935929321,-0.527065809433042));
#9175=CARTESIAN_POINT('Ctrl Pts',(0.640559927378796,0.718104410331526,-0.147019361766098));
#9176=CARTESIAN_POINT('Ctrl Pts',(0.537831107754837,0.738736997373318,0.373647816694899));
#9177=CARTESIAN_POINT('Ctrl Pts',(0.0845805647471646,0.759259943025514,
0.645113960140173));
#9178=CARTESIAN_POINT('Ctrl Pts',(-0.281268703654681,0.774162449469679,
0.535302832262414));
#9179=CARTESIAN_POINT('Ctrl Pts',(-0.437006958245047,0.783485974077427,
0.378958889142701));
#9180=CARTESIAN_POINT('Ctrl Pts',(-0.507697370885022,0.788549978506264,
0.281850016683051));
#9181=CARTESIAN_POINT('Ctrl Pts',(-0.590811263696918,0.79755702495982,0.0865772474568527));
#9182=CARTESIAN_POINT('Ctrl Pts',(-0.570421542490006,0.807404168621158,
-0.163998512585474));
#9183=CARTESIAN_POINT('Ctrl Pts',(-0.449519165229382,0.817962511928117,
-0.368907152618757));
#9184=CARTESIAN_POINT('Ctrl Pts',(-0.331434707315454,0.823631825677829,
-0.470158335662351));
#9185=CARTESIAN_POINT('Ctrl Pts',(-0.228414168702972,0.828869835105896,
-0.524261354796639));
#9186=CARTESIAN_POINT('Ctrl Pts',(-0.124409789837836,0.83479670994367,-0.559486616067973));
#9187=CARTESIAN_POINT('Ctrl Pts',(0.0311860121700488,0.84127032933758,-0.573462474344531));
#9188=CARTESIAN_POINT('Ctrl Pts',(0.286930207599112,0.839831852204138,-0.56941247728844));
#9189=CARTESIAN_POINT('Ctrl Pts',(0.544368769266695,0.837758405835724,-0.566662924739702));
#9190=CARTESIAN_POINT('Ctrl Pts',(0.77915350747992,0.839083640925069,-0.568525018908883));
#9191=CARTESIAN_POINT('Ctrl Pts',(1.10406134980889,0.839169583354872,-0.568697614612765));
#9192=CARTESIAN_POINT('Ctrl Pts',(1.51463887381527,0.838547420648682,-0.567751119234392));
#9193=CARTESIAN_POINT('Ctrl Pts',(1.83619420925238,0.839098369729373,-0.568574422943627));
#9194=CARTESIAN_POINT('Ctrl Pts',(2.0000345343157,0.838924340696319,-0.568319470976886));
#9195=CARTESIAN_POINT('Ctrl Pts',(0.62672943408441,0.0786682492038075,-1.99995803330129));
#9196=CARTESIAN_POINT('Ctrl Pts',(0.626984281206633,0.0784942917339065,
-1.83618507879303));
#9197=CARTESIAN_POINT('Ctrl Pts',(0.626167881567446,0.0790457108498767,
-1.51485561868953));
#9198=CARTESIAN_POINT('Ctrl Pts',(0.627102473829725,0.0784231080938741,
-1.10373920604851));
#9199=CARTESIAN_POINT('Ctrl Pts',(0.626949240460296,0.0785101683511648,
-0.779449572693693));
#9200=CARTESIAN_POINT('Ctrl Pts',(0.625050745785335,0.0798328338465923,
-0.544462149089626));
#9201=CARTESIAN_POINT('Ctrl Pts',(0.627889985740265,0.0777656623793459,
-0.285696293823589));
#9202=CARTESIAN_POINT('Ctrl Pts',(0.631738128714664,0.0763139712887997,
-0.0328999352935243));
#9203=CARTESIAN_POINT('Ctrl Pts',(0.618203355232202,0.0828217339857707,
0.126016338436061));
#9204=CARTESIAN_POINT('Ctrl Pts',(0.5788696130134,0.089502164873538,0.243540471625212));
#9205=CARTESIAN_POINT('Ctrl Pts',(0.518429935075775,0.0953194797976742,
0.357975889465943));
#9206=CARTESIAN_POINT('Ctrl Pts',(0.4085463000272,0.10148208753481,0.486163680166641));
#9207=CARTESIAN_POINT('Ctrl Pts',(0.18454758337479,0.112981193016189,0.618576938164562));
#9208=CARTESIAN_POINT('Ctrl Pts',(-0.154217959045931,0.126437065904357,
0.644731550026875));
#9209=CARTESIAN_POINT('Ctrl Pts',(-0.53919139895456,0.144820634753371,0.407325706570045));
#9210=CARTESIAN_POINT('Ctrl Pts',(-0.686206851627058,0.164726032742826,
-0.0832228853543702));
#9211=CARTESIAN_POINT('Ctrl Pts',(-0.398055690096881,0.186466555625688,
-0.561844820235381));
#9212=CARTESIAN_POINT('Ctrl Pts',(0.10085458709022,0.206247303003531,-0.659997015644472));
#9213=CARTESIAN_POINT('Ctrl Pts',(0.482784624497038,0.224177467621409,-0.432799283114279));
#9214=CARTESIAN_POINT('Ctrl Pts',(0.642581592200899,0.240248144748989,-0.0691618097941696));
#9215=CARTESIAN_POINT('Ctrl Pts',(0.559567552302235,0.256264600472695,0.318623559236399));
#9216=CARTESIAN_POINT('Ctrl Pts',(0.266823917287717,0.272221182924003,0.583443542472237));
#9217=CARTESIAN_POINT('Ctrl Pts',(-0.124194342342738,0.288120357516062,
0.62698047179839));
#9218=CARTESIAN_POINT('Ctrl Pts',(-0.465474692842472,0.303961011116931,
0.434750176991032));
#9219=CARTESIAN_POINT('Ctrl Pts',(-0.629665991844459,0.319743666769981,
0.0797039890484459));
#9220=CARTESIAN_POINT('Ctrl Pts',(-0.563291828984184,0.333721066643941,
-0.25863406390321));
#9221=CARTESIAN_POINT('Ctrl Pts',(-0.317177505535178,0.349397283704289,
-0.546449972718228));
#9222=CARTESIAN_POINT('Ctrl Pts',(0.0716126775062496,0.365015623748908,
-0.639472176834321));
#9223=CARTESIAN_POINT('Ctrl Pts',(0.44843287350778,0.382294855949406,-0.434852100630385));
#9224=CARTESIAN_POINT('Ctrl Pts',(0.63574682531925,0.399510275598109,-0.0530429731296652));
#9225=CARTESIAN_POINT('Ctrl Pts',(0.504663248626496,0.418366227351729,0.414638002521349));
#9226=CARTESIAN_POINT('Ctrl Pts',(0.0859614245310279,0.436560993262288,
0.620946393148274));
#9227=CARTESIAN_POINT('Ctrl Pts',(-0.292431686101597,0.452416791448528,
0.531200841970267));
#9228=CARTESIAN_POINT('Ctrl Pts',(-0.526265761537412,0.465963442852263,
0.29684552061805));
#9229=CARTESIAN_POINT('Ctrl Pts',(-0.615560796465379,0.481716911656766,
-0.0792565511246861));
#9230=CARTESIAN_POINT('Ctrl Pts',(-0.410344088232626,0.499648879780982,
-0.490947805481661));
#9231=CARTESIAN_POINT('Ctrl Pts',(0.0871079884122845,0.519725898932142,
-0.630875565640356));
#9232=CARTESIAN_POINT('Ctrl Pts',(0.522394114004133,0.539708055100366,-0.35851478036304));
#9233=CARTESIAN_POINT('Ctrl Pts',(0.614106517526869,0.55959700282496,0.144195500945888));
#9234=CARTESIAN_POINT('Ctrl Pts',(0.304551390300492,0.57939424257321,0.548632718489485));
#9235=CARTESIAN_POINT('Ctrl Pts',(-0.143262545090784,0.596911693363567,
0.587123558035457));
#9236=CARTESIAN_POINT('Ctrl Pts',(-0.450004619985209,0.612182310173313,
0.371935416025931));
#9237=CARTESIAN_POINT('Ctrl Pts',(-0.577120807453118,0.62523280671009,0.079266601333838));
#9238=CARTESIAN_POINT('Ctrl Pts',(-0.530462301562817,0.638245507692561,
-0.236320918010667));
#9239=CARTESIAN_POINT('Ctrl Pts',(-0.32526663056702,0.651220933950828,-0.479186888619294));
#9240=CARTESIAN_POINT('Ctrl Pts',(-0.0241756368245449,0.66415927198707,
-0.576609424925001));
#9241=CARTESIAN_POINT('Ctrl Pts',(0.334495973140524,0.679212452857298,-0.489701096053415));
#9242=CARTESIAN_POINT('Ctrl Pts',(0.596200424927635,0.696356179648218,-0.136231806846881));
#9243=CARTESIAN_POINT('Ctrl Pts',(0.500642690062709,0.715568736684096,0.348576033177884));
#9244=CARTESIAN_POINT('Ctrl Pts',(0.0782134587988113,0.734699394529406,
0.601783229446777));
#9245=CARTESIAN_POINT('Ctrl Pts',(-0.263334440263774,0.74861335220138,0.499309887430558));
#9246=CARTESIAN_POINT('Ctrl Pts',(-0.408761144108869,0.75731773364333,0.353356897942407));
#9247=CARTESIAN_POINT('Ctrl Pts',(-0.474830525070825,0.762054113932951,
0.262524775384885));
#9248=CARTESIAN_POINT('Ctrl Pts',(-0.552641913792421,0.770463016151057,
0.0802325505851415));
#9249=CARTESIAN_POINT('Ctrl Pts',(-0.533212125162727,0.779701800604458,
-0.154774313380276));
#9250=CARTESIAN_POINT('Ctrl Pts',(-0.420511229514612,0.789556784600691,
-0.345980730976801));
#9251=CARTESIAN_POINT('Ctrl Pts',(-0.309815844486922,0.794867133309828,
-0.440969276372039));
#9252=CARTESIAN_POINT('Ctrl Pts',(-0.212711168959734,0.799809791402836,
-0.491916344579349));
#9253=CARTESIAN_POINT('Ctrl Pts',(-0.116675449236811,0.805274071611186,
-0.524469634945247));
#9254=CARTESIAN_POINT('Ctrl Pts',(0.0312001431979104,0.811517204070306,
-0.538144006859143));
#9255=CARTESIAN_POINT('Ctrl Pts',(0.285951855836605,0.810147186315183,-0.534168979189779));
#9256=CARTESIAN_POINT('Ctrl Pts',(0.544362350217127,0.808042230889924,-0.531389671259308));
#9257=CARTESIAN_POINT('Ctrl Pts',(0.77960272849961,0.809380172550063,-0.533265960326483));
#9258=CARTESIAN_POINT('Ctrl Pts',(1.10367239586754,0.80945930366762,-0.533432761018123));
#9259=CARTESIAN_POINT('Ctrl Pts',(1.51493665542971,0.808841636111715,-0.532492980025066));
#9260=CARTESIAN_POINT('Ctrl Pts',(1.83618388576743,0.809390251128783,-0.533315228872414));
#9261=CARTESIAN_POINT('Ctrl Pts',(1.99994811217411,0.809216302926719,-0.53306039532281));
#9262=CARTESIAN_POINT('Ctrl Pts',(0.5874609188711,0.0822019824159158,-1.99989317407337));
#9263=CARTESIAN_POINT('Ctrl Pts',(0.587715677265367,0.0820280855113077,
-1.83617723900198));
#9264=CARTESIAN_POINT('Ctrl Pts',(0.58689971250081,0.0825772844454769,-1.51508654260829));
#9265=CARTESIAN_POINT('Ctrl Pts',(0.587831000225384,0.0819585874321892,
-1.10344749883076));
#9266=CARTESIAN_POINT('Ctrl Pts',(0.587680460234937,0.0820393800455694,
-0.779804611248477));
#9267=CARTESIAN_POINT('Ctrl Pts',(0.585775499994469,0.083373568561431,-0.544448425778546));
#9268=CARTESIAN_POINT('Ctrl Pts',(0.58862845690685,0.0812774489656124,-0.285022784695781));
#9269=CARTESIAN_POINT('Ctrl Pts',(0.592441914962544,0.079888127716253,-0.0326774653733658));
#9270=CARTESIAN_POINT('Ctrl Pts',(0.579108229824713,0.086188207924076,0.11900070157323));
#9271=CARTESIAN_POINT('Ctrl Pts',(0.542704406423502,0.0923562996112714,
0.227612687921699));
#9272=CARTESIAN_POINT('Ctrl Pts',(0.485928138725982,0.0978317117759704,
0.335239816192948));
#9273=CARTESIAN_POINT('Ctrl Pts',(0.382789952176369,0.103609371928733,0.455495129550219));
#9274=CARTESIAN_POINT('Ctrl Pts',(0.173445112617297,0.114358088999672,0.579131350820057));
#9275=CARTESIAN_POINT('Ctrl Pts',(-0.144342710046836,0.126982880344674,
0.603964833450006));
#9276=CARTESIAN_POINT('Ctrl Pts',(-0.504617540795482,0.144187615680568,
0.381427965458317));
#9277=CARTESIAN_POINT('Ctrl Pts',(-0.642383911453795,0.162830042168221,
-0.0777436199891682));
#9278=CARTESIAN_POINT('Ctrl Pts',(-0.372578271513367,0.18317769756345,-0.525811039595045));
#9279=CARTESIAN_POINT('Ctrl Pts',(0.0943497013842308,0.201692512692434,
-0.617644888618581));
#9280=CARTESIAN_POINT('Ctrl Pts',(0.451815269396865,0.218473010441523,-0.405014599643461));
#9281=CARTESIAN_POINT('Ctrl Pts',(0.601373785637953,0.233514060494329,-0.0646699181159046));
#9282=CARTESIAN_POINT('Ctrl Pts',(0.523679013910274,0.248505254417583,0.29829880585065));
#9283=CARTESIAN_POINT('Ctrl Pts',(0.24964403741173,0.263442115335976,0.546206089476511));
#9284=CARTESIAN_POINT('Ctrl Pts',(-0.116451337731323,0.278327625975953,
0.586979022297046));
#9285=CARTESIAN_POINT('Ctrl Pts',(-0.436054891647266,0.29316158596241,0.406974772591184));
#9286=CARTESIAN_POINT('Ctrl Pts',(-0.589870298345399,0.30794504129165,0.0744078582288452));
#9287=CARTESIAN_POINT('Ctrl Pts',(-0.527692943172682,0.321041534993931,
-0.242618792914012));
#9288=CARTESIAN_POINT('Ctrl Pts',(-0.297023701829149,0.335734465321562,
-0.512391077873751));
#9289=CARTESIAN_POINT('Ctrl Pts',(0.0675212641741527,0.35037904755484,-0.5996538147588));
#9290=CARTESIAN_POINT('Ctrl Pts',(0.421056594556602,0.366589258750743,-0.407716742702501));
#9291=CARTESIAN_POINT('Ctrl Pts',(0.596905393478329,0.382748228505995,-0.0493501504687293));
#9292=CARTESIAN_POINT('Ctrl Pts',(0.473862910947153,0.400458116239252,0.389940683934648));
#9293=CARTESIAN_POINT('Ctrl Pts',(0.0802903162289862,0.417561901608528,
0.583953158059964));
#9294=CARTESIAN_POINT('Ctrl Pts',(-0.275709966682282,0.432478726710855,
0.499557870740994));
#9295=CARTESIAN_POINT('Ctrl Pts',(-0.495862448390292,0.445231474030675,
0.278949853677765));
#9296=CARTESIAN_POINT('Ctrl Pts',(-0.580023400465553,0.46007217823348,-0.0753512915820435));
#9297=CARTESIAN_POINT('Ctrl Pts',(-0.386607022200923,0.476980336558612,
-0.463591036362349));
#9298=CARTESIAN_POINT('Ctrl Pts',(0.0829877251595423,0.495934135576676,
-0.595818995283933));
#9299=CARTESIAN_POINT('Ctrl Pts',(0.494534882711716,0.514822618485088,-0.338472445755909));
#9300=CARTESIAN_POINT('Ctrl Pts',(0.581491499979929,0.533648931251995,0.137363743733339));
#9301=CARTESIAN_POINT('Ctrl Pts',(0.288161264391336,0.552415905203638,0.52085580206473));
#9302=CARTESIAN_POINT('Ctrl Pts',(-0.137003162728498,0.569047439534844,
0.557541558510368));
#9303=CARTESIAN_POINT('Ctrl Pts',(-0.428676822886062,0.583565633440864,
0.352995905254951));
#9304=CARTESIAN_POINT('Ctrl Pts',(-0.549711004700905,0.595987212241011,
0.0744483287800028));
#9305=CARTESIAN_POINT('Ctrl Pts',(-0.505299948228852,0.608386728377244,
-0.226282687840735));
#9306=CARTESIAN_POINT('Ctrl Pts',(-0.309575039133742,0.620765578833677,
-0.45802323172802));
#9307=CARTESIAN_POINT('Ctrl Pts',(-0.0219755772339618,0.633124488893754,
-0.551129760420029));
#9308=CARTESIAN_POINT('Ctrl Pts',(0.321081796479251,0.647521942421836,-0.468075339341517));
#9309=CARTESIAN_POINT('Ctrl Pts',(0.571917008721482,0.663944142090889,-0.129561094078861));
#9310=CARTESIAN_POINT('Ctrl Pts',(0.480393018973127,0.682387090247801,0.335843108412934));
#9311=CARTESIAN_POINT('Ctrl Pts',(0.0741693531238315,0.700787378825874,
0.57961025567971));
#9312=CARTESIAN_POINT('Ctrl Pts',(-0.255143275996557,0.714201786052559,
0.480937271720544));
#9313=CARTESIAN_POINT('Ctrl Pts',(-0.395498171738189,0.722601182697331,
0.340100684060336));
#9314=CARTESIAN_POINT('Ctrl Pts',(-0.459314101410141,0.727177877012928,
0.252326763909831));
#9315=CARTESIAN_POINT('Ctrl Pts',(-0.534583243568393,0.735297491050186,
0.0763204025504257));
#9316=CARTESIAN_POINT('Ctrl Pts',(-0.515616512133595,0.7442503799837,-0.151391320167515));
#9317=CARTESIAN_POINT('Ctrl Pts',(-0.406711704651741,0.753781299451576,
-0.336277015933739));
#9318=CARTESIAN_POINT('Ctrl Pts',(-0.299435189638348,0.758923960221984,
-0.428370572052981));
#9319=CARTESIAN_POINT('Ctrl Pts',(-0.204694398152886,0.763750096791064,
-0.47808447397292));
#9320=CARTESIAN_POINT('Ctrl Pts',(-0.112050112984815,0.769013820539994,
-0.509451539857503));
#9321=CARTESIAN_POINT('Ctrl Pts',(0.0314195100887834,0.775117938261012,
-0.522885083062355));
#9322=CARTESIAN_POINT('Ctrl Pts',(0.285217271752917,0.773788624023985,-0.518977616945277));
#9323=CARTESIAN_POINT('Ctrl Pts',(0.544377275887181,0.7716647254831,-0.516167687470469));
#9324=CARTESIAN_POINT('Ctrl Pts',(0.77992084130335,0.773010147661079,-0.518055833052231));
#9325=CARTESIAN_POINT('Ctrl Pts',(1.10339956738025,0.773085111411238,-0.518215860268804));
#9326=CARTESIAN_POINT('Ctrl Pts',(1.51514747628628,0.772470044939352,-0.517280005423198));
#9327=CARTESIAN_POINT('Ctrl Pts',(1.83617635170566,0.773017182662106,-0.518099756538723));
#9328=CARTESIAN_POINT('Ctrl Pts',(1.99988580057488,0.77284329264402,-0.517845008228458));
#9329=CARTESIAN_POINT('Ctrl Pts',(0.550945450866199,0.067105092762305,-1.99985238806428));
#9330=CARTESIAN_POINT('Ctrl Pts',(0.551200153361326,0.0669312340141922,
-1.83617237557771));
#9331=CARTESIAN_POINT('Ctrl Pts',(0.550383059047253,0.067478738759276,-1.51523700162691));
#9332=CARTESIAN_POINT('Ctrl Pts',(0.551312121940096,0.0668631648982134,
-1.10325776056893));
#9333=CARTESIAN_POINT('Ctrl Pts',(0.551160834485697,0.0669390897119991,
-0.780037484764116));
#9334=CARTESIAN_POINT('Ctrl Pts',(0.549254306488641,0.0682824421640895,
-0.544421315854621));
#9335=CARTESIAN_POINT('Ctrl Pts',(0.552106416364749,0.0661635755354553,
-0.284639224380358));
#9336=CARTESIAN_POINT('Ctrl Pts',(0.555914749094926,0.0648235660252144,
-0.0323032591833498));
#9337=CARTESIAN_POINT('Ctrl Pts',(0.542682333476631,0.0709613521230218,
0.11348170634836));
#9338=CARTESIAN_POINT('Ctrl Pts',(0.508977099615909,0.0766537088572853,
0.213768678876433));
#9339=CARTESIAN_POINT('Ctrl Pts',(0.455708834950571,0.0818026163180467,
0.314916823094266));
#9340=CARTESIAN_POINT('Ctrl Pts',(0.358692386569373,0.0872323354600932,
0.427975224214404));
#9341=CARTESIAN_POINT('Ctrl Pts',(0.162663694190769,0.097298924680809,0.543646775182899));
#9342=CARTESIAN_POINT('Ctrl Pts',(-0.136192113262965,0.109174509901586,
0.567305343826758));
#9343=CARTESIAN_POINT('Ctrl Pts',(-0.474558443064967,0.125332340697949,
0.358045956782264));
#9344=CARTESIAN_POINT('Ctrl Pts',(-0.60433801784961,0.142871565376813,-0.0736684299162183));
#9345=CARTESIAN_POINT('Ctrl Pts',(-0.350381954033981,0.162024342912799,
-0.495576784770102));
#9346=CARTESIAN_POINT('Ctrl Pts',(0.0896117759143228,0.179474692463962,
-0.582204390142572));
#9347=CARTESIAN_POINT('Ctrl Pts',(0.426885853840544,0.195305136977579,-0.381668836262442));
#9348=CARTESIAN_POINT('Ctrl Pts',(0.568149223251883,0.20950819707601,-0.0603124683763491));
#9349=CARTESIAN_POINT('Ctrl Pts',(0.494770009110161,0.22367796540124,0.282770658933988));
#9350=CARTESIAN_POINT('Ctrl Pts',(0.235528087739685,0.237810882245137,0.517373264212428));
#9351=CARTESIAN_POINT('Ctrl Pts',(-0.111222533228894,0.251910335567996,
0.556051654550424));
#9352=CARTESIAN_POINT('Ctrl Pts',(-0.414313232539064,0.265976879461039,
0.385418487215813));
#9353=CARTESIAN_POINT('Ctrl Pts',(-0.560401318983622,0.280011870110238,
0.0697231995474879));
#9354=CARTESIAN_POINT('Ctrl Pts',(-0.501352286024681,0.292460599828054,
-0.231630199439596));
#9355=CARTESIAN_POINT('Ctrl Pts',(-0.281902903004944,0.306441274341836,
-0.488339555795956));
#9356=CARTESIAN_POINT('Ctrl Pts',(0.065387266285567,0.320393957968718,-0.571596489894968));
#9357=CARTESIAN_POINT('Ctrl Pts',(0.402799127650896,0.335863029162657,-0.388516285439416));
#9358=CARTESIAN_POINT('Ctrl Pts',(0.570909994761135,0.351304546428848,-0.0461096493466856));
#9359=CARTESIAN_POINT('Ctrl Pts',(0.453309975606592,0.368257239503034,0.374426206306753));
#9360=CARTESIAN_POINT('Ctrl Pts',(0.0759001441926504,0.384661798048627,
0.560666086673735));
#9361=CARTESIAN_POINT('Ctrl Pts',(-0.266151455502317,0.398993403813706,
0.479651913020883));
#9362=CARTESIAN_POINT('Ctrl Pts',(-0.478001702726463,0.411263096833331,
0.267441030022521));
#9363=CARTESIAN_POINT('Ctrl Pts',(-0.55916305232678,0.425562184968444,-0.0738989456599627));
#9364=CARTESIAN_POINT('Ctrl Pts',(-0.372636699601196,0.441883583112284,
-0.448734050354975));
#9365=CARTESIAN_POINT('Ctrl Pts',(0.0816035926774441,0.460220680465181,
-0.576880646792149));
#9366=CARTESIAN_POINT('Ctrl Pts',(0.480801224099281,0.478537007133273,-0.327530135042584));
#9367=CARTESIAN_POINT('Ctrl Pts',(0.565551782967983,0.496836451246379,0.134930498293982));
#9368=CARTESIAN_POINT('Ctrl Pts',(0.279939442908263,0.515122401597484,0.508738501339385));
#9369=CARTESIAN_POINT('Ctrl Pts',(-0.135321607217399,0.5313675615131,0.544776075890801));
#9370=CARTESIAN_POINT('Ctrl Pts',(-0.420872324450394,0.54557805985139,0.344637404158902));
#9371=CARTESIAN_POINT('Ctrl Pts',(-0.539596413905804,0.557756821355681,
0.071564075139448));
#9372=CARTESIAN_POINT('Ctrl Pts',(-0.496054610193741,0.569935034483373,
-0.223801635132005));
#9373=CARTESIAN_POINT('Ctrl Pts',(-0.303551962745066,0.582113820788074,
-0.451841305044243));
#9374=CARTESIAN_POINT('Ctrl Pts',(-0.0201376858984327,0.594293856531097,
-0.543665136012608));
#9375=CARTESIAN_POINT('Ctrl Pts',(0.318550684880049,0.608507626299889,-0.461760947931387));
#9376=CARTESIAN_POINT('Ctrl Pts',(0.56690994352398,0.624756550847024,-0.126963600293733));
#9377=CARTESIAN_POINT('Ctrl Pts',(0.47637525653217,0.643052724327624,0.334766757063998));
#9378=CARTESIAN_POINT('Ctrl Pts',(0.0724483648226123,0.661355498523464,
0.577485257188254));
#9379=CARTESIAN_POINT('Ctrl Pts',(-0.256055153330988,0.674735290731573,
0.479237459957281));
#9380=CARTESIAN_POINT('Ctrl Pts',(-0.396261391483261,0.683125208503875,
0.338563008491415));
#9381=CARTESIAN_POINT('Ctrl Pts',(-0.460044070922385,0.687699882890572,
0.250826790073639));
#9382=CARTESIAN_POINT('Ctrl Pts',(-0.535356310780212,0.695820111538706,
0.0748271639382049));
#9383=CARTESIAN_POINT('Ctrl Pts',(-0.51637969164712,0.704791213538561,-0.153359389343171));
#9384=CARTESIAN_POINT('Ctrl Pts',(-0.407166121656258,0.714351503734276,
-0.338801256616131));
#9385=CARTESIAN_POINT('Ctrl Pts',(-0.299604806090809,0.7195056868629,-0.431148288532543));
#9386=CARTESIAN_POINT('Ctrl Pts',(-0.20397209222849,0.724379105857744,-0.481389271359994));
#9387=CARTESIAN_POINT('Ctrl Pts',(-0.110498436078102,0.729684445910484,
-0.512948589891693));
#9388=CARTESIAN_POINT('Ctrl Pts',(0.0317754025745838,0.73573981334391,-0.526218953561026));
#9389=CARTESIAN_POINT('Ctrl Pts',(0.284730439464858,0.734424495251457,-0.522371841874736));
#9390=CARTESIAN_POINT('Ctrl Pts',(0.544396269643961,0.732294283957779,-0.519536512654844));
#9391=CARTESIAN_POINT('Ctrl Pts',(0.780091402972714,0.73364230094729,-0.521435851662876));
#9392=CARTESIAN_POINT('Ctrl Pts',(1.10324034467337,0.733715868350949,-0.521590658029006));
#9393=CARTESIAN_POINT('Ctrl Pts',(1.51526428502092,0.733101852305696,-0.520659208592313));
#9394=CARTESIAN_POINT('Ctrl Pts',(1.83617199619976,0.73364855145534,-0.521477483502039));
#9395=CARTESIAN_POINT('Ctrl Pts',(1.9998492399299,0.733474695645128,-0.521222785306198));
#9396=CARTESIAN_POINT('Ctrl Pts',(0.534004674862244,0.0469900053766836,
-1.99984739250011));
#9397=CARTESIAN_POINT('Ctrl Pts',(0.534259370517448,0.0468161512974708,
-1.83617177556803));
#9398=CARTESIAN_POINT('Ctrl Pts',(0.533441502311306,0.047363056988596,-1.51526191633464));
#9399=CARTESIAN_POINT('Ctrl Pts',(0.534371434639262,0.0467484424255759,
-1.10323146349633));
#9400=CARTESIAN_POINT('Ctrl Pts',(0.53421824455692,0.0468227288278506,-0.780080082057997));
#9401=CARTESIAN_POINT('Ctrl Pts',(0.53231508003366,0.0481691265924268,-0.5444042631695));
#9402=CARTESIAN_POINT('Ctrl Pts',(0.53515856794429,0.0460425754822485,-0.284643294266451));
#9403=CARTESIAN_POINT('Ctrl Pts',(0.538985648847748,0.0447190117196379,
-0.0320211294696051));
#9404=CARTESIAN_POINT('Ctrl Pts',(0.525741686811735,0.0508034693757587,
0.111631344947843));
#9405=CARTESIAN_POINT('Ctrl Pts',(0.493267866324073,0.0562760720192935,
0.208037659421039));
#9406=CARTESIAN_POINT('Ctrl Pts',(0.441696713730458,0.0612676600297227,
0.306080548947707));
#9407=CARTESIAN_POINT('Ctrl Pts',(0.347410886319535,0.0665431383971926,
0.415933050789519));
#9408=CARTESIAN_POINT('Ctrl Pts',(0.157327861273452,0.0763049024739723,
0.528057489188086));
#9409=CARTESIAN_POINT('Ctrl Pts',(-0.133156674943477,0.0878492851954371,
0.551209324434459));
#9410=CARTESIAN_POINT('Ctrl Pts',(-0.462129068607569,0.103556824422786,
0.347710166812253));
#9411=CARTESIAN_POINT('Ctrl Pts',(-0.588638599629634,0.120634315916664,
-0.0725030008931035));
#9412=CARTESIAN_POINT('Ctrl Pts',(-0.341164585828511,0.139304871497971,
-0.483904151910011));
#9413=CARTESIAN_POINT('Ctrl Pts',(0.0883544884891012,0.15634168137637,-0.568597044331401));
#9414=CARTESIAN_POINT('Ctrl Pts',(0.418095753693205,0.171816150349456,-0.372629793275881));
#9415=CARTESIAN_POINT('Ctrl Pts',(0.556391570690854,0.185715675527505,-0.0581644462312985));
#9416=CARTESIAN_POINT('Ctrl Pts',(0.484561146319725,0.199598451089136,0.277982796567569));
#9417=CARTESIAN_POINT('Ctrl Pts',(0.230314847899877,0.213461297531163,0.508150230707778));
#9418=CARTESIAN_POINT('Ctrl Pts',(-0.110207364221293,0.227307713902608,
0.546197798579722));
#9419=CARTESIAN_POINT('Ctrl Pts',(-0.408248667614897,0.241138498233169,
0.378481405677519));
#9420=CARTESIAN_POINT('Ctrl Pts',(-0.55212786122253,0.254955114808116,0.0677253194967843));
#9421=CARTESIAN_POINT('Ctrl Pts',(-0.493976322541745,0.267225343790709,
-0.229320675962668));
#9422=CARTESIAN_POINT('Ctrl Pts',(-0.277480263691582,0.281019977096165,
-0.482633192044066));
#9423=CARTESIAN_POINT('Ctrl Pts',(0.065596463336222,0.294804411465538,-0.564997000764067));
#9424=CARTESIAN_POINT('Ctrl Pts',(0.399482932950473,0.310109780450929,-0.38392530822993));
#9425=CARTESIAN_POINT('Ctrl Pts',(0.56609494129569,0.325407661924638,-0.0447422502843249));
#9426=CARTESIAN_POINT('Ctrl Pts',(0.449568840578391,0.342228227329634,0.372555088313464));
#9427=CARTESIAN_POINT('Ctrl Pts',(0.0745015920546068,0.358533475231174,
0.557805153430069));
#9428=CARTESIAN_POINT('Ctrl Pts',(-0.265999568209032,0.372799304426681,
0.477222072678098));
#9429=CARTESIAN_POINT('Ctrl Pts',(-0.477158534899731,0.385027113765151,
0.265766140699257));
#9430=CARTESIAN_POINT('Ctrl Pts',(-0.55819880007667,0.399294294380163,-0.0747901036973868));
#9431=CARTESIAN_POINT('Ctrl Pts',(-0.371948198635926,0.41560348526982,-0.4494077686762));
#9432=CARTESIAN_POINT('Ctrl Pts',(0.0827104291202138,0.433959582494683,
-0.577860783198243));
#9433=CARTESIAN_POINT('Ctrl Pts',(0.483129998632293,0.452327631229365,-0.327955043863337));
#9434=CARTESIAN_POINT('Ctrl Pts',(0.568442679422367,0.47071146405326,0.13660223562247));
#9435=CARTESIAN_POINT('Ctrl Pts',(0.281144892082092,0.489114336526312,0.51291059653611));
#9436=CARTESIAN_POINT('Ctrl Pts',(-0.137494533186177,0.50549224525999,0.549390016718285));
#9437=CARTESIAN_POINT('Ctrl Pts',(-0.425840925255912,0.519839749453121,
0.347369191128545));
#9438=CARTESIAN_POINT('Ctrl Pts',(-0.545888211304912,0.53215017858499,0.0713630548919239));
#9439=CARTESIAN_POINT('Ctrl Pts',(-0.50187537147456,0.544474304440711,-0.227546071152447));
#9440=CARTESIAN_POINT('Ctrl Pts',(-0.306881264535124,0.556813096530318,
-0.458613263717583));
#9441=CARTESIAN_POINT('Ctrl Pts',(-0.0194326697730112,0.569167100060671,
-0.551791152038062));
#9442=CARTESIAN_POINT('Ctrl Pts',(0.324485383771089,0.583600014619787,-0.46868203399731));
#9443=CARTESIAN_POINT('Ctrl Pts',(0.57713540063447,0.600122698894204,-0.12833611767096));
#9444=CARTESIAN_POINT('Ctrl Pts',(0.485092061602979,0.618757114787167,0.341960480204146));
#9445=CARTESIAN_POINT('Ctrl Pts',(0.0731066834054238,0.637429046052168,
0.589705029297371));
#9446=CARTESIAN_POINT('Ctrl Pts',(-0.262559945489057,0.651098951528179,
0.489439247431335));
#9447=CARTESIAN_POINT('Ctrl Pts',(-0.40596163751793,0.659680303032932,0.345554732462302));
#9448=CARTESIAN_POINT('Ctrl Pts',(-0.47120314927041,0.664358692530949,0.255830744517815));
#9449=CARTESIAN_POINT('Ctrl Pts',(-0.548255068766781,0.672671758647096,
0.0756627500398241));
#9450=CARTESIAN_POINT('Ctrl Pts',(-0.528961115138206,0.681853354797658,
-0.157915933389433));
#9451=CARTESIAN_POINT('Ctrl Pts',(-0.41686144719521,0.691663500854672,-0.348212222865038));
#9452=CARTESIAN_POINT('Ctrl Pts',(-0.306694249169893,0.696942448975099,
-0.442778117175704));
#9453=CARTESIAN_POINT('Ctrl Pts',(-0.208440137034481,0.701948967530146,
-0.494458985485184));
#9454=CARTESIAN_POINT('Ctrl Pts',(-0.111735576307102,0.707436605013493,
-0.527032573056622));
#9455=CARTESIAN_POINT('Ctrl Pts',(0.0320564404187695,0.713526797401297,
-0.540268761905287));
#9456=CARTESIAN_POINT('Ctrl Pts',(0.284651256534309,0.712200783188229,-0.53644652612564));
#9457=CARTESIAN_POINT('Ctrl Pts',(0.544412867618483,0.710075632452311,-0.533600539455794));
#9458=CARTESIAN_POINT('Ctrl Pts',(0.780083942590528,0.711421670395101,-0.535504501896504));
#9459=CARTESIAN_POINT('Ctrl Pts',(1.10323653929954,0.711496312658999,-0.535657095037923));
#9460=CARTESIAN_POINT('Ctrl Pts',(1.51526257912182,0.710881717500948,-0.534727266050874));
#9461=CARTESIAN_POINT('Ctrl Pts',(1.83617179277114,0.711428825678065,-0.535544837400977));
#9462=CARTESIAN_POINT('Ctrl Pts',(1.99984752864807,0.711254971469475,-0.535290141551507));
#9463=CARTESIAN_POINT('Ctrl Pts',(0.528325516000818,0.0355351383793534,
-1.99985072236852));
#9464=CARTESIAN_POINT('Ctrl Pts',(0.528580216238454,0.0353612811721935,
-1.83617216061816));
#9465=CARTESIAN_POINT('Ctrl Pts',(0.527761919981528,0.0359080598807752,
-1.51525401386864));
#9466=CARTESIAN_POINT('Ctrl Pts',(0.528692709166738,0.0352936010092843,
-1.10324464383216));
#9467=CARTESIAN_POINT('Ctrl Pts',(0.528538249039279,0.0353675670609071,
-0.780070492797932));
#9468=CARTESIAN_POINT('Ctrl Pts',(0.526637602108816,0.0367145593105412,
-0.544396520018928));
#9469=CARTESIAN_POINT('Ctrl Pts',(0.529475094326102,0.0345864750367511,
-0.284709647833573));
#9470=CARTESIAN_POINT('Ctrl Pts',(0.533315915563189,0.0332661260171643,
-0.0318866342588667));
#9471=CARTESIAN_POINT('Ctrl Pts',(0.520046729613095,0.0393406257213133,
0.111267345674666));
#9472=CARTESIAN_POINT('Ctrl Pts',(0.487978555806356,0.0447398499197174,
0.206365118213754));
#9473=CARTESIAN_POINT('Ctrl Pts',(0.437001774418032,0.0496765590551313,
0.303330442803063));
#9474=CARTESIAN_POINT('Ctrl Pts',(0.34359217210679,0.054902908379379,0.412155588816351));
#9475=CARTESIAN_POINT('Ctrl Pts',(0.155419901809077,0.064566620841489,0.523143450471739));
#9476=CARTESIAN_POINT('Ctrl Pts',(-0.132406193515106,0.076005890905876,
0.5461393872929));
#9477=CARTESIAN_POINT('Ctrl Pts',(-0.4585052544005,0.0915751768415844,0.344428446786955));
#9478=CARTESIAN_POINT('Ctrl Pts',(-0.584075679141621,0.108515922097861,
-0.0723729196787201));
#9479=CARTESIAN_POINT('Ctrl Pts',(-0.338462248411882,0.12705070506418,-0.480836123882888));
#9480=CARTESIAN_POINT('Ctrl Pts',(0.0882708030427006,0.143977745088325,
-0.565053420420048));
#9481=CARTESIAN_POINT('Ctrl Pts',(0.416146086422155,0.159363348118548,-0.370243292897184));
#9482=CARTESIAN_POINT('Ctrl Pts',(0.553763732742827,0.173191747342348,-0.0573989645046387));
#9483=CARTESIAN_POINT('Ctrl Pts',(0.482289890064134,0.18701212633461,0.277245974053173));
#9484=CARTESIAN_POINT('Ctrl Pts',(0.229047329307677,0.200821415024854,0.506551175681503));
#9485=CARTESIAN_POINT('Ctrl Pts',(-0.110374003483933,0.214623123412753,
0.544510067179701));
#9486=CARTESIAN_POINT('Ctrl Pts',(-0.40766150283296,0.228418090582837,0.377257404939042));
#9487=CARTESIAN_POINT('Ctrl Pts',(-0.551295150396298,0.242207808252135,
0.0671188908067961));
#9488=CARTESIAN_POINT('Ctrl Pts',(-0.493245643443692,0.254462036591453,
-0.229548648448914));
#9489=CARTESIAN_POINT('Ctrl Pts',(-0.276929936242163,0.268246205655378,
-0.48268043415828));
#9490=CARTESIAN_POINT('Ctrl Pts',(0.0660979817878402,0.282029157249401,
-0.56509208661935));
#9491=CARTESIAN_POINT('Ctrl Pts',(0.400224908210924,0.297344357665888,-0.383938719179592));
#9492=CARTESIAN_POINT('Ctrl Pts',(0.567086603737135,0.312662109365757,-0.0443326451316622));
#9493=CARTESIAN_POINT('Ctrl Pts',(0.450399697790572,0.329517044874313,0.373843214320543));
#9494=CARTESIAN_POINT('Ctrl Pts',(0.0742631586112486,0.34586991722832,0.559702372303342));
#9495=CARTESIAN_POINT('Ctrl Pts',(-0.267488833499262,0.360187667101961,
0.478855140322724));
#9496=CARTESIAN_POINT('Ctrl Pts',(-0.479552956006764,0.37246695090628,0.266522113563231));
#9497=CARTESIAN_POINT('Ctrl Pts',(-0.561010089555589,0.386802304605621,
-0.0756527104584505));
#9498=CARTESIAN_POINT('Ctrl Pts',(-0.37380142743242,0.40320076618434,-0.45235567176097));
#9499=CARTESIAN_POINT('Ctrl Pts',(0.0837105500021586,0.421672872730665,
-0.581703055845243));
#9500=CARTESIAN_POINT('Ctrl Pts',(0.487040755149608,0.44017222169388,-0.330077148654899));
#9501=CARTESIAN_POINT('Ctrl Pts',(0.573113162045742,0.458702465869511,0.138170100375564));
#9502=CARTESIAN_POINT('Ctrl Pts',(0.28335615351346,0.477266726235763,0.517831802862951));
#9503=CARTESIAN_POINT('Ctrl Pts',(-0.139284333173075,0.493801248027276,
0.55472840308304));
#9504=CARTESIAN_POINT('Ctrl Pts',(-0.430595948725319,0.508295268527237,
0.350662848554826));
#9505=CARTESIAN_POINT('Ctrl Pts',(-0.551949910444459,0.520737729754399,
0.0717040146871301));
#9506=CARTESIAN_POINT('Ctrl Pts',(-0.507464290067291,0.533200036194741,
-0.230562528994356));
#9507=CARTESIAN_POINT('Ctrl Pts',(-0.31020166413149,0.545683273612848,-0.464351384435429));
#9508=CARTESIAN_POINT('Ctrl Pts',(-0.0192492650129703,0.558188014622219,
-0.558684300589107));
#9509=CARTESIAN_POINT('Ctrl Pts',(0.329035122965687,0.572803913266816,-0.474545710915398));
#9510=CARTESIAN_POINT('Ctrl Pts',(0.585077648306754,0.589545384238961,-0.129724768044979));
#9511=CARTESIAN_POINT('Ctrl Pts',(0.49182251269281,0.608439403717184,0.347142406791056));
#9512=CARTESIAN_POINT('Ctrl Pts',(0.0738519459812565,0.627383860376655,
0.598553246116509));
#9513=CARTESIAN_POINT('Ctrl Pts',(-0.26692557334338,0.641260854247049,0.496816287527571));
#9514=CARTESIAN_POINT('Ctrl Pts',(-0.412574454609541,0.649976893163681,
0.350671912292324));
#9515=CARTESIAN_POINT('Ctrl Pts',(-0.478836302760905,0.654727738162907,
0.259559307243844));
#9516=CARTESIAN_POINT('Ctrl Pts',(-0.557090734433065,0.663174756391869,
0.0764917316856528));
#9517=CARTESIAN_POINT('Ctrl Pts',(-0.537578911396685,0.672499276473955,
-0.160750767756091));
#9518=CARTESIAN_POINT('Ctrl Pts',(-0.423523769730798,0.682478242160259,
-0.354329770148811));
#9519=CARTESIAN_POINT('Ctrl Pts',(-0.311592602102818,0.687841923158427,
-0.450394818907249));
#9520=CARTESIAN_POINT('Ctrl Pts',(-0.211664235020424,0.692933107210186,
-0.502988933683848));
#9521=CARTESIAN_POINT('Ctrl Pts',(-0.11285095039931,0.698540582073528,-0.536235596855463));
#9522=CARTESIAN_POINT('Ctrl Pts',(0.0321957650443905,0.704663061559795,
-0.549474282988733));
#9523=CARTESIAN_POINT('Ctrl Pts',(0.284679981111006,0.70332721476915,-0.545658664585203));
#9524=CARTESIAN_POINT('Ctrl Pts',(0.544423010813361,0.701206594196697,-0.542808989660773));
#9525=CARTESIAN_POINT('Ctrl Pts',(0.780051600334079,0.702550794007654,-0.544713980589938));
#9526=CARTESIAN_POINT('Ctrl Pts',(1.10326148850366,0.702626394058564,-0.544865639596336));
#9527=CARTESIAN_POINT('Ctrl Pts',(1.51524226187871,0.702011181204639,-0.543935752090523));
#9528=CARTESIAN_POINT('Ctrl Pts',(1.83617236681158,0.702558621549799,-0.544752786768393));
#9529=CARTESIAN_POINT('Ctrl Pts',(1.9998524353109,0.702384762739154,-0.544498084176928));
#9530=CARTESIAN_POINT('',(1.9998524353109,0.702384762739154,-0.544498084176928));
#9531=CARTESIAN_POINT('',(0.528325516000818,0.0355351383793534,-1.99985072236852));
#9532=CARTESIAN_POINT('Ctrl Pts',(1.9998524353109,0.702384762739154,-0.544498084176928));
#9533=CARTESIAN_POINT('Ctrl Pts',(1.83617236681158,0.702558621549799,-0.544752786768393));
#9534=CARTESIAN_POINT('Ctrl Pts',(1.51524226187871,0.702011181204639,-0.543935752090523));
#9535=CARTESIAN_POINT('Ctrl Pts',(1.10326148850366,0.702626394058564,-0.544865639596336));
#9536=CARTESIAN_POINT('Ctrl Pts',(0.780051600334079,0.702550794007654,-0.544713980589938));
#9537=CARTESIAN_POINT('Ctrl Pts',(0.544423010813361,0.701206594196697,-0.542808989660773));
#9538=CARTESIAN_POINT('Ctrl Pts',(0.284679981111006,0.70332721476915,-0.545658664585203));
#9539=CARTESIAN_POINT('Ctrl Pts',(0.0321957650443905,0.704663061559795,
-0.549474282988733));
#9540=CARTESIAN_POINT('Ctrl Pts',(-0.11285095039931,0.698540582073528,-0.536235596855463));
#9541=CARTESIAN_POINT('Ctrl Pts',(-0.211664235020424,0.692933107210186,
-0.502988933683848));
#9542=CARTESIAN_POINT('Ctrl Pts',(-0.311592602102818,0.687841923158427,
-0.450394818907249));
#9543=CARTESIAN_POINT('Ctrl Pts',(-0.423523769730798,0.682478242160259,
-0.354329770148811));
#9544=CARTESIAN_POINT('Ctrl Pts',(-0.537578911396685,0.672499276473955,
-0.160750767756091));
#9545=CARTESIAN_POINT('Ctrl Pts',(-0.557090734433065,0.663174756391869,
0.0764917316856528));
#9546=CARTESIAN_POINT('Ctrl Pts',(-0.478836302760905,0.654727738162907,
0.259559307243844));
#9547=CARTESIAN_POINT('Ctrl Pts',(-0.412574454609541,0.649976893163681,
0.350671912292324));
#9548=CARTESIAN_POINT('Ctrl Pts',(-0.26692557334338,0.641260854247049,0.496816287527571));
#9549=CARTESIAN_POINT('Ctrl Pts',(0.0738519459812565,0.627383860376655,
0.598553246116509));
#9550=CARTESIAN_POINT('Ctrl Pts',(0.49182251269281,0.608439403717184,0.347142406791056));
#9551=CARTESIAN_POINT('Ctrl Pts',(0.585077648306754,0.589545384238961,-0.129724768044979));
#9552=CARTESIAN_POINT('Ctrl Pts',(0.329035122965687,0.572803913266816,-0.474545710915398));
#9553=CARTESIAN_POINT('Ctrl Pts',(-0.0192492650129703,0.558188014622219,
-0.558684300589107));
#9554=CARTESIAN_POINT('Ctrl Pts',(-0.31020166413149,0.545683273612848,-0.464351384435429));
#9555=CARTESIAN_POINT('Ctrl Pts',(-0.507464290067291,0.533200036194741,
-0.230562528994356));
#9556=CARTESIAN_POINT('Ctrl Pts',(-0.551949910444459,0.520737729754399,
0.0717040146871301));
#9557=CARTESIAN_POINT('Ctrl Pts',(-0.430595948725319,0.508295268527237,
0.350662848554826));
#9558=CARTESIAN_POINT('Ctrl Pts',(-0.139284333173075,0.493801248027276,
0.55472840308304));
#9559=CARTESIAN_POINT('Ctrl Pts',(0.28335615351346,0.477266726235763,0.517831802862951));
#9560=CARTESIAN_POINT('Ctrl Pts',(0.573113162045742,0.458702465869511,0.138170100375564));
#9561=CARTESIAN_POINT('Ctrl Pts',(0.487040755149608,0.44017222169388,-0.330077148654899));
#9562=CARTESIAN_POINT('Ctrl Pts',(0.0837105500021586,0.421672872730665,
-0.581703055845243));
#9563=CARTESIAN_POINT('Ctrl Pts',(-0.37380142743242,0.40320076618434,-0.45235567176097));
#9564=CARTESIAN_POINT('Ctrl Pts',(-0.561010089555589,0.386802304605621,
-0.0756527104584505));
#9565=CARTESIAN_POINT('Ctrl Pts',(-0.479552956006764,0.37246695090628,0.266522113563231));
#9566=CARTESIAN_POINT('Ctrl Pts',(-0.267488833499262,0.360187667101961,
0.478855140322724));
#9567=CARTESIAN_POINT('Ctrl Pts',(0.0742631586112486,0.34586991722832,0.559702372303342));
#9568=CARTESIAN_POINT('Ctrl Pts',(0.450399697790572,0.329517044874313,0.373843214320543));
#9569=CARTESIAN_POINT('Ctrl Pts',(0.567086603737135,0.312662109365757,-0.0443326451316622));
#9570=CARTESIAN_POINT('Ctrl Pts',(0.400224908210924,0.297344357665888,-0.383938719179592));
#9571=CARTESIAN_POINT('Ctrl Pts',(0.0660979817878402,0.282029157249401,
-0.56509208661935));
#9572=CARTESIAN_POINT('Ctrl Pts',(-0.276929936242163,0.268246205655378,
-0.48268043415828));
#9573=CARTESIAN_POINT('Ctrl Pts',(-0.493245643443692,0.254462036591453,
-0.229548648448914));
#9574=CARTESIAN_POINT('Ctrl Pts',(-0.551295150396298,0.242207808252135,
0.0671188908067961));
#9575=CARTESIAN_POINT('Ctrl Pts',(-0.40766150283296,0.228418090582837,0.377257404939042));
#9576=CARTESIAN_POINT('Ctrl Pts',(-0.110374003483933,0.214623123412753,
0.544510067179701));
#9577=CARTESIAN_POINT('Ctrl Pts',(0.229047329307677,0.200821415024854,0.506551175681503));
#9578=CARTESIAN_POINT('Ctrl Pts',(0.482289890064134,0.18701212633461,0.277245974053173));
#9579=CARTESIAN_POINT('Ctrl Pts',(0.553763732742827,0.173191747342348,-0.0573989645046387));
#9580=CARTESIAN_POINT('Ctrl Pts',(0.416146086422155,0.159363348118548,-0.370243292897184));
#9581=CARTESIAN_POINT('Ctrl Pts',(0.0882708030427006,0.143977745088325,
-0.565053420420048));
#9582=CARTESIAN_POINT('Ctrl Pts',(-0.338462248411882,0.12705070506418,-0.480836123882888));
#9583=CARTESIAN_POINT('Ctrl Pts',(-0.584075679141621,0.108515922097861,
-0.0723729196787201));
#9584=CARTESIAN_POINT('Ctrl Pts',(-0.4585052544005,0.0915751768415844,0.344428446786955));
#9585=CARTESIAN_POINT('Ctrl Pts',(-0.132406193515106,0.076005890905876,
0.5461393872929));
#9586=CARTESIAN_POINT('Ctrl Pts',(0.155419901809077,0.064566620841489,0.523143450471739));
#9587=CARTESIAN_POINT('Ctrl Pts',(0.34359217210679,0.054902908379379,0.412155588816351));
#9588=CARTESIAN_POINT('Ctrl Pts',(0.437001774418032,0.0496765590551313,
0.303330442803063));
#9589=CARTESIAN_POINT('Ctrl Pts',(0.487978555806356,0.0447398499197174,
0.206365118213754));
#9590=CARTESIAN_POINT('Ctrl Pts',(0.520046729613095,0.0393406257213133,
0.111267345674666));
#9591=CARTESIAN_POINT('Ctrl Pts',(0.533315915563189,0.0332661260171643,
-0.0318866342588667));
#9592=CARTESIAN_POINT('Ctrl Pts',(0.529475094326102,0.0345864750367511,
-0.284709647833573));
#9593=CARTESIAN_POINT('Ctrl Pts',(0.526637602108816,0.0367145593105412,
-0.544396520018928));
#9594=CARTESIAN_POINT('Ctrl Pts',(0.528538249039279,0.0353675670609071,
-0.780070492797932));
#9595=CARTESIAN_POINT('Ctrl Pts',(0.528692709166738,0.0352936010092843,
-1.10324464383216));
#9596=CARTESIAN_POINT('Ctrl Pts',(0.527761919981528,0.0359080598807752,
-1.51525401386864));
#9597=CARTESIAN_POINT('Ctrl Pts',(0.528580216238454,0.0353612811721935,
-1.83617216061816));
#9598=CARTESIAN_POINT('Ctrl Pts',(0.528325516000818,0.0355351383793534,
-1.99985072236852));
#9599=CARTESIAN_POINT('',(2.00015071794412,0.804475523135573,-0.666497406911305));
#9600=CARTESIAN_POINT('Origin',(1.99999999999998,0.759999999999999,-0.60000000000007));
#9601=CARTESIAN_POINT('',(0.662463988280159,-0.0499822726657336,-2.00015029073282));
#9602=CARTESIAN_POINT('Ctrl Pts',(2.00015071794412,0.804475523135573,-0.666497406911305));
#9603=CARTESIAN_POINT('Ctrl Pts',(1.83620821687538,0.804649660698633,-0.66675251787415));
#9604=CARTESIAN_POINT('Ctrl Pts',(1.51421119194035,0.804093904068503,-0.665928948647562));
#9605=CARTESIAN_POINT('Ctrl Pts',(1.10459263968738,0.804724235202262,-0.66687751216757));
#9606=CARTESIAN_POINT('Ctrl Pts',(0.778488091977107,0.804624888614752,-0.666703265676913));
#9607=CARTESIAN_POINT('Ctrl Pts',(0.54442707625171,0.8033242699894,-0.664844003722482));
#9608=CARTESIAN_POINT('Ctrl Pts',(0.288027302850487,0.805335668320584,-0.667586118918959));
#9609=CARTESIAN_POINT('Ctrl Pts',(0.0321180206196141,0.806907294366097,
-0.671653874643804));
#9610=CARTESIAN_POINT('Ctrl Pts',(-0.139596638836966,0.799988366367406,
-0.657366153595634));
#9611=CARTESIAN_POINT('Ctrl Pts',(-0.265956682682317,0.792781771671027,
-0.614881276898037));
#9612=CARTESIAN_POINT('Ctrl Pts',(-0.386340473147736,0.786669200591926,
-0.551372175845378));
#9613=CARTESIAN_POINT('Ctrl Pts',(-0.523816993927788,0.780063785948551,
-0.433645748061385));
#9614=CARTESIAN_POINT('Ctrl Pts',(-0.666219044663549,0.767653433960867,
-0.192704218915611));
#9615=CARTESIAN_POINT('Ctrl Pts',(-0.689058767063034,0.756222082569521,
0.0984146554749596));
#9616=CARTESIAN_POINT('Ctrl Pts',(-0.592478248153049,0.74570751472679,0.326342499792088));
#9617=CARTESIAN_POINT('Ctrl Pts',(-0.510250580429896,0.739824441432273,
0.439145396424497));
#9618=CARTESIAN_POINT('Ctrl Pts',(-0.328971586153759,0.728968689390915,
0.621190836988033));
#9619=CARTESIAN_POINT('Ctrl Pts',(0.0958337440893244,0.711671376372341,
0.74830999711301));
#9620=CARTESIAN_POINT('Ctrl Pts',(0.620304111002753,0.687911568470837,0.433769461113443));
#9621=CARTESIAN_POINT('Ctrl Pts',(0.73835387107679,0.664111160627632,-0.166965130048199));
#9622=CARTESIAN_POINT('Ctrl Pts',(0.414715655942592,0.642922729480766,-0.603621999120373));
#9623=CARTESIAN_POINT('Ctrl Pts',(-0.0275908863199736,0.62436100859898,
-0.710669286038228));
#9624=CARTESIAN_POINT('Ctrl Pts',(-0.39813025511233,0.608437064253082,-0.590670145737896));
#9625=CARTESIAN_POINT('Ctrl Pts',(-0.650080156703408,0.592499998475874,
-0.292288521076879));
#9626=CARTESIAN_POINT('Ctrl Pts',(-0.707144881750632,0.57655098007586,0.0945309854926571));
#9627=CARTESIAN_POINT('Ctrl Pts',(-0.55158365946692,0.56059094898577,0.452401551542145));
#9628=CARTESIAN_POINT('Ctrl Pts',(-0.1772094561828,0.541959207305282,0.714834645121414));
#9629=CARTESIAN_POINT('Ctrl Pts',(0.367484330759339,0.520650735211898,0.667598289986901));
#9630=CARTESIAN_POINT('Ctrl Pts',(0.742175157663465,0.496662180030771,0.177201798791322));
#9631=CARTESIAN_POINT('Ctrl Pts',(0.630965640778732,0.472660315479601,-0.429375166251397));
#9632=CARTESIAN_POINT('Ctrl Pts',(0.107586035230619,0.448648433132338,-0.756188390862319));
#9633=CARTESIAN_POINT('Ctrl Pts',(-0.487350453008389,0.424630334656425,
-0.588208599365547));
#9634=CARTESIAN_POINT('Ctrl Pts',(-0.731235197502955,0.403278517609434,
-0.0977683708505558));
#9635=CARTESIAN_POINT('Ctrl Pts',(-0.625117601034868,0.384596133557627,
0.348183842295094));
#9636=CARTESIAN_POINT('Ctrl Pts',(-0.348606790473969,0.368583951861805,
0.625079898555237));
#9637=CARTESIAN_POINT('Ctrl Pts',(0.0972167907293641,0.34990603829391,0.730574719890591));
#9638=CARTESIAN_POINT('Ctrl Pts',(0.588086029972563,0.328565375698038,0.488053495238463));
#9639=CARTESIAN_POINT('Ctrl Pts',(0.740365136709862,0.306568406437996,-0.0577085025886233));
#9640=CARTESIAN_POINT('Ctrl Pts',(0.522621279421028,0.286581789189134,-0.500819963452499));
#9641=CARTESIAN_POINT('Ctrl Pts',(0.0867941523773002,0.266605918529927,
-0.737064913155744));
#9642=CARTESIAN_POINT('Ctrl Pts',(-0.36030002070441,0.248640851668397,-0.629569645495563));
#9643=CARTESIAN_POINT('Ctrl Pts',(-0.641992299862074,0.230688881084643,
-0.299876917809462));
#9644=CARTESIAN_POINT('Ctrl Pts',(-0.717478987054585,0.214742051156983,
0.086194632105411));
#9645=CARTESIAN_POINT('Ctrl Pts',(-0.530690929834931,0.196817259725453,
0.489300976461692));
#9646=CARTESIAN_POINT('Ctrl Pts',(-0.144725676703892,0.178909769816401,
0.70633098622582));
#9647=CARTESIAN_POINT('Ctrl Pts',(0.295215046776041,0.161020056779893,0.657018975821946));
#9648=CARTESIAN_POINT('Ctrl Pts',(0.622824528841228,0.143151007884386,0.360207879087552));
#9649=CARTESIAN_POINT('Ctrl Pts',(0.715006044039375,0.125301300434412,-0.0720347673296787));
#9650=CARTESIAN_POINT('Ctrl Pts',(0.53747991286649,0.107478289621193,-0.475188997283933));
#9651=CARTESIAN_POINT('Ctrl Pts',(0.115758946274973,0.0876905285771165,
-0.725599039992233));
#9652=CARTESIAN_POINT('Ctrl Pts',(-0.431538112822807,0.0659892634348224,
-0.617104732797172));
#9653=CARTESIAN_POINT('Ctrl Pts',(-0.744693743478759,0.0422927786570434,
-0.0951523515529584));
#9654=CARTESIAN_POINT('Ctrl Pts',(-0.585085784735021,0.0207569079373872,
0.435755076168825));
#9655=CARTESIAN_POINT('Ctrl Pts',(-0.170310845287768,0.00096264921625724,
0.690490277729099));
#9656=CARTESIAN_POINT('Ctrl Pts',(0.191480329024041,-0.0134075415523006,
0.662765347245377));
#9657=CARTESIAN_POINT('Ctrl Pts',(0.431002395435098,-0.0256993836631372,
0.520971575878654));
#9658=CARTESIAN_POINT('Ctrl Pts',(0.548065973192159,-0.032280894159065,
0.384307758714896));
#9659=CARTESIAN_POINT('Ctrl Pts',(0.611163697009464,-0.0383525034286994,
0.264648815779984));
#9660=CARTESIAN_POINT('Ctrl Pts',(0.65335380658105,-0.0455068140358546,
0.139218056313768));
#9661=CARTESIAN_POINT('Ctrl Pts',(0.667640080240138,-0.0524139639419364,
-0.0320317672708526));
#9662=CARTESIAN_POINT('Ctrl Pts',(0.663563470597623,-0.0508446374556383,
-0.288026483088336));
#9663=CARTESIAN_POINT('Ctrl Pts',(0.660820022877162,-0.0488315955858374,
-0.544415125004604));
#9664=CARTESIAN_POINT('Ctrl Pts',(0.662676266642772,-0.050132523365314,
-0.778488486630415));
#9665=CARTESIAN_POINT('Ctrl Pts',(0.662849183916153,-0.050231417425612,
-1.10458538375921));
#9666=CARTESIAN_POINT('Ctrl Pts',(0.661897332210143,-0.0496009500256405,
-1.51421284590545));
#9667=CARTESIAN_POINT('Ctrl Pts',(0.662719098649113,-0.050156409826639,
-1.8362081654112));
#9668=CARTESIAN_POINT('Ctrl Pts',(0.662463988280159,-0.0499822726657336,
-2.00015029073282));
#9669=CARTESIAN_POINT('Origin',(0.6,0.,-2.));
#9670=CARTESIAN_POINT('Ctrl Pts',(0.600124355483126,-0.0799998580128369,
-2.00008516830249));
#9671=CARTESIAN_POINT('Ctrl Pts',(0.600379376695518,-0.0801739343158842,
-1.83620033785433));
#9672=CARTESIAN_POINT('Ctrl Pts',(0.599562611053881,-0.0796184124528264,
-1.5144754520526));
#9673=CARTESIAN_POINT('Ctrl Pts',(0.600502518404447,-0.0802525034314073,
-1.10424411057565));
#9674=CARTESIAN_POINT('Ctrl Pts',(0.600344602427935,-0.0801506833161176,
-0.778901942331774));
#9675=CARTESIAN_POINT('Ctrl Pts',(0.598456953704134,-0.0788587712934794,
-0.544242160533997));
#9676=CARTESIAN_POINT('Ctrl Pts',(0.601272474507003,-0.0808543685860998,
-0.287680267082095));
#9677=CARTESIAN_POINT('Ctrl Pts',(0.605184477979747,-0.0824681761820383,
-0.0307556431383126));
#9678=CARTESIAN_POINT('Ctrl Pts',(0.588609512632607,-0.0742202560328195,
0.161001223625551));
#9679=CARTESIAN_POINT('Ctrl Pts',(0.518063450209372,-0.0648906358873938,
0.323627369018429));
#9680=CARTESIAN_POINT('Ctrl Pts',(0.389740128736442,-0.0579722786893707,
0.474748184678881));
#9681=CARTESIAN_POINT('Ctrl Pts',(0.173020606908044,-0.0467144436845919,
0.602178110487582));
#9682=CARTESIAN_POINT('Ctrl Pts',(-0.156647509262585,-0.0336993466160229,
0.628366170043479));
#9683=CARTESIAN_POINT('Ctrl Pts',(-0.534302969503257,-0.01563383198389,
0.396152535345114));
#9684=CARTESIAN_POINT('Ctrl Pts',(-0.680181221263981,0.00400588873282267,
-0.0887030397692518));
#9685=CARTESIAN_POINT('Ctrl Pts',(-0.465603142330848,0.0202821362637637,
-0.446134214125788));
#9686=CARTESIAN_POINT('Ctrl Pts',(-0.165486932860075,0.03474270768116,-0.612245575240685));
#9687=CARTESIAN_POINT('Ctrl Pts',(0.146295095787791,0.0474352484480225,
-0.642641412885972));
#9688=CARTESIAN_POINT('Ctrl Pts',(0.495949774692522,0.0637997238881112,
-0.436123139243827));
#9689=CARTESIAN_POINT('Ctrl Pts',(0.659385538859151,0.0802233041204479,
-0.0644782106763051));
#9690=CARTESIAN_POINT('Ctrl Pts',(0.574545201045043,0.0966991572901908,
0.334449484668907));
#9691=CARTESIAN_POINT('Ctrl Pts',(0.271532605139402,0.113229721085999,0.609171048717871));
#9692=CARTESIAN_POINT('Ctrl Pts',(-0.136251969463658,0.129813195665052,
0.654997123118035));
#9693=CARTESIAN_POINT('Ctrl Pts',(-0.494901592911036,0.146449576154649,
0.453502429895765));
#9694=CARTESIAN_POINT('Ctrl Pts',(-0.668917284177339,0.163138203343486,
0.0782620703516101));
#9695=CARTESIAN_POINT('Ctrl Pts',(-0.598644996586867,0.178018517289954,
-0.282046799603755));
#9696=CARTESIAN_POINT('Ctrl Pts',(-0.335262243900907,0.194801447000121,
-0.590258574308657));
#9697=CARTESIAN_POINT('Ctrl Pts',(0.0833281156314849,0.211635077569448,
-0.691395156339746));
#9698=CARTESIAN_POINT('Ctrl Pts',(0.4320119853653,0.227588446215705,-0.502587368796631));
#9699=CARTESIAN_POINT('Ctrl Pts',(0.58527223262087,0.238874211068699,-0.281979562605746));
#9700=CARTESIAN_POINT('Ctrl Pts',(0.678917739338141,0.252059849462334,0.0184388692246381));
#9701=CARTESIAN_POINT('Ctrl Pts',(0.554821413577227,0.270001502682695,0.463024783480917));
#9702=CARTESIAN_POINT('Ctrl Pts',(0.089888824047859,0.290221470828933,0.693551038003489));
#9703=CARTESIAN_POINT('Ctrl Pts',(-0.272915151999609,0.305432097922516,
0.607393400489082));
#9704=CARTESIAN_POINT('Ctrl Pts',(-0.465626168527264,0.315590515005467,
0.46173311346713));
#9705=CARTESIAN_POINT('Ctrl Pts',(-0.611423927492396,0.325760833794014,
0.268821318511434));
#9706=CARTESIAN_POINT('Ctrl Pts',(-0.698650473779508,0.341042831595186,
-0.0956472554953462));
#9707=CARTESIAN_POINT('Ctrl Pts',(-0.465321982498693,0.361476665326508,
-0.565350807747607));
#9708=CARTESIAN_POINT('Ctrl Pts',(0.10575120321005,0.38454069790763,-0.726974188805798));
#9709=CARTESIAN_POINT('Ctrl Pts',(0.610387251745808,0.407678360873112,-0.412408779209339));
#9710=CARTESIAN_POINT('Ctrl Pts',(0.718323895495084,0.430887045922702,0.17413060542287));
#9711=CARTESIAN_POINT('Ctrl Pts',(0.355237119019683,0.454164351458316,0.650683811024646));
#9712=CARTESIAN_POINT('Ctrl Pts',(-0.175382406590221,0.4749142230429,0.695878649309196));
#9713=CARTESIAN_POINT('Ctrl Pts',(-0.54101475967607,0.49311138275633,0.440269492223299));
#9714=CARTESIAN_POINT('Ctrl Pts',(-0.693527526572458,0.50873629806685,0.0898379898580044));
#9715=CARTESIAN_POINT('Ctrl Pts',(-0.646735970560938,0.521779183073869,
-0.226461651899009));
#9716=CARTESIAN_POINT('Ctrl Pts',(-0.513906112786406,0.532226370805735,
-0.436433419735239));
#9717=CARTESIAN_POINT('Ctrl Pts',(-0.328920782360512,0.542681936352062,
-0.602852159734885));
#9718=CARTESIAN_POINT('Ctrl Pts',(-0.0243494995865983,0.55576702001899,
-0.701905622444322));
#9719=CARTESIAN_POINT('Ctrl Pts',(0.318684360355662,0.570182439320145,-0.618057422392217));
#9720=CARTESIAN_POINT('Ctrl Pts',(0.554275268889935,0.583304705413154,-0.407908493988256));
#9721=CARTESIAN_POINT('Ctrl Pts',(0.713586310862138,0.599067032359038,-0.0629718800249659));
#9722=CARTESIAN_POINT('Ctrl Pts',(0.617323759198901,0.61880473745743,0.433855029903579));
#9723=CARTESIAN_POINT('Ctrl Pts',(0.0931818027763926,0.642526983889894,
0.749181117386836));
#9724=CARTESIAN_POINT('Ctrl Pts',(-0.314313763037281,0.659133011706964,
0.627311226200405));
#9725=CARTESIAN_POINT('Ctrl Pts',(-0.477269723836412,0.668539639010893,
0.476341934975343));
#9726=CARTESIAN_POINT('Ctrl Pts',(-0.524957853949116,0.671513213020625,
0.424882768662061));
#9727=CARTESIAN_POINT('Ctrl Pts',(-0.597179322807005,0.676677358782867,
0.325569816011966));
#9728=CARTESIAN_POINT('Ctrl Pts',(-0.69448376569806,0.6873032670482,0.0964041117283874));
#9729=CARTESIAN_POINT('Ctrl Pts',(-0.671478747098358,0.69869719950028,-0.197322255866813));
#9730=CARTESIAN_POINT('Ctrl Pts',(-0.527686488423399,0.711441182605667,
-0.440569074748579));
#9731=CARTESIAN_POINT('Ctrl Pts',(-0.36114955668007,0.719020822056164,-0.583433135906584));
#9732=CARTESIAN_POINT('Ctrl Pts',(-0.171544666302877,0.729888896055897,
-0.664752607658936));
#9733=CARTESIAN_POINT('Ctrl Pts',(0.0327819626725445,0.738541246775484,
-0.681326463162123));
#9734=CARTESIAN_POINT('Ctrl Pts',(0.287281763425397,0.736796378226309,-0.677467579294977));
#9735=CARTESIAN_POINT('Ctrl Pts',(0.544477498698488,0.734860197456536,-0.674632411152923));
#9736=CARTESIAN_POINT('Ctrl Pts',(0.778765801010588,0.736127346477361,-0.676530344298986));
#9737=CARTESIAN_POINT('Ctrl Pts',(1.10435275137728,0.736241519844584,-0.676684603908725));
#9738=CARTESIAN_POINT('Ctrl Pts',(1.51439530422594,0.735599108498541,-0.675749139626198));
#9739=CARTESIAN_POINT('Ctrl Pts',(1.83620130898864,0.736158775205915,-0.676565295388702));
#9740=CARTESIAN_POINT('Ctrl Pts',(2.00009323767342,0.735984691360175,-0.676310263121555));
#9741=CARTESIAN_POINT('Ctrl Pts',(0.623974753147584,-0.0799627443810934,
-2.00012224248872));
#9742=CARTESIAN_POINT('Ctrl Pts',(0.624229825439503,-0.0801368555507905,
-1.83620458669381));
#9743=CARTESIAN_POINT('Ctrl Pts',(0.623412063162941,-0.0795796261306918,
-1.51433796979021));
#9744=CARTESIAN_POINT('Ctrl Pts',(0.624359859480197,-0.0802179503669397,
-1.10443039061536));
#9745=CARTESIAN_POINT('Ctrl Pts',(0.62419562566126,-0.0801105878584707,
-0.778694387346514));
#9746=CARTESIAN_POINT('Ctrl Pts',(0.622325145889363,-0.0788301395864106,
-0.544301413101009));
#9747=CARTESIAN_POINT('Ctrl Pts',(0.625106583269737,-0.0807989774146498,
-0.288007276047959));
#9748=CARTESIAN_POINT('Ctrl Pts',(0.629104794486704,-0.0824730503396987,
-0.031111740534322));
#9749=CARTESIAN_POINT('Ctrl Pts',(0.612250467993575,-0.0740274841813297,
0.166374233370359));
#9750=CARTESIAN_POINT('Ctrl Pts',(0.538550980620464,-0.0642460178139413,
0.336780746391469));
#9751=CARTESIAN_POINT('Ctrl Pts',(0.405452154198712,-0.057098070267831,
0.493123831974176));
#9752=CARTESIAN_POINT('Ctrl Pts',(0.179790463925493,-0.045362414675718,
0.626129196125436));
#9753=CARTESIAN_POINT('Ctrl Pts',(-0.162515835153933,-0.0318610350483913,
0.652948899440053));
#9754=CARTESIAN_POINT('Ctrl Pts',(-0.555104121078402,-0.013076772153776,
0.411861924804563));
#9755=CARTESIAN_POINT('Ctrl Pts',(-0.706494995716607,0.00731586852288217,
-0.0919341536269851));
#9756=CARTESIAN_POINT('Ctrl Pts',(-0.483689317242129,0.0242199786601462,
-0.463046839212734));
#9757=CARTESIAN_POINT('Ctrl Pts',(-0.172085161128402,0.0392327419485987,
-0.635510782103407));
#9758=CARTESIAN_POINT('Ctrl Pts',(0.151534851775174,0.0524067893783082,
-0.667051829582526));
#9759=CARTESIAN_POINT('Ctrl Pts',(0.514342017305476,0.0693857790668076,
-0.452740521293047));
#9760=CARTESIAN_POINT('Ctrl Pts',(0.68385146227568,0.0864208989509592,-0.0672288061262263));
#9761=CARTESIAN_POINT('Ctrl Pts',(0.595856693475746,0.103503527696193,0.346416299319125));
#9762=CARTESIAN_POINT('Ctrl Pts',(0.281766337021811,0.120636343208791,0.631146960462356));
#9763=CARTESIAN_POINT('Ctrl Pts',(-0.140730452143404,0.137816821820559,
0.67859963752343));
#9764=CARTESIAN_POINT('Ctrl Pts',(-0.512143481669323,0.15504448338329,0.469904875349947));
#9765=CARTESIAN_POINT('Ctrl Pts',(-0.692248298424958,0.172318474499937,
0.0814608902124625));
#9766=CARTESIAN_POINT('Ctrl Pts',(-0.619518631402499,0.187712934444724,
-0.291320794134974));
#9767=CARTESIAN_POINT('Ctrl Pts',(-0.347101977382683,0.205069580874819,
-0.610083796980475));
#9768=CARTESIAN_POINT('Ctrl Pts',(0.0856264740795014,0.222470485013252,
-0.714571021120727));
#9769=CARTESIAN_POINT('Ctrl Pts',(0.44580046722091,0.238948816751437,-0.519495022345486));
#9770=CARTESIAN_POINT('Ctrl Pts',(0.604066108994964,0.25060297477869,-0.291675312775178));
#9771=CARTESIAN_POINT('Ctrl Pts',(0.700738910463294,0.264215420555072,0.0184849426418081));
#9772=CARTESIAN_POINT('Ctrl Pts',(0.572640898984596,0.282723178790392,0.477162825367339));
#9773=CARTESIAN_POINT('Ctrl Pts',(0.0932568014054071,0.303568974758758,
0.714756971115007));
#9774=CARTESIAN_POINT('Ctrl Pts',(-0.280540254320519,0.319240073683042,
0.625960485616185));
#9775=CARTESIAN_POINT('Ctrl Pts',(-0.479004310712579,0.32970135829011,0.47594246027192));
#9776=CARTESIAN_POINT('Ctrl Pts',(-0.629123425868339,0.340173193562948,
0.277305322213801));
#9777=CARTESIAN_POINT('Ctrl Pts',(-0.718857967185726,0.355898871371537,
-0.0977904793576591));
#9778=CARTESIAN_POINT('Ctrl Pts',(-0.478821925431186,0.376910052425976,
-0.580774275577745));
#9779=CARTESIAN_POINT('Ctrl Pts',(0.107973512819069,0.40060519253458,-0.746719455522737));
#9780=CARTESIAN_POINT('Ctrl Pts',(0.625924802892503,0.424354169765414,-0.423710203648399));
#9781=CARTESIAN_POINT('Ctrl Pts',(0.736504811271342,0.448152928948129,0.177837918946914));
#9782=CARTESIAN_POINT('Ctrl Pts',(0.36440052610237,0.471999615636857,0.666006076478248));
#9783=CARTESIAN_POINT('Ctrl Pts',(-0.178677986430279,0.493233270995688,
0.712167492060102));
#9784=CARTESIAN_POINT('Ctrl Pts',(-0.552580736158049,0.511842586077471,
0.450719359413262));
#9785=CARTESIAN_POINT('Ctrl Pts',(-0.708421284622368,0.527810293363266,
0.0925696490070121));
#9786=CARTESIAN_POINT('Ctrl Pts',(-0.660610117307273,0.541126816837653,
-0.230412043824339));
#9787=CARTESIAN_POINT('Ctrl Pts',(-0.525019612582926,0.551790527195324,
-0.444737715779806));
#9788=CARTESIAN_POINT('Ctrl Pts',(-0.336266792259839,0.562457991275901,
-0.6145419193976));
#9789=CARTESIAN_POINT('Ctrl Pts',(-0.0256559250583661,0.575801054431563,
-0.715518174515178));
#9790=CARTESIAN_POINT('Ctrl Pts',(0.323914068012285,0.590490635965341,-0.630042052906425));
#9791=CARTESIAN_POINT('Ctrl Pts',(0.563820115939216,0.603852583815099,-0.416011490533624));
#9792=CARTESIAN_POINT('Ctrl Pts',(0.725951907577493,0.619896011193044,-0.0648918311942802));
#9793=CARTESIAN_POINT('Ctrl Pts',(0.627947962839659,0.639966556187965,0.440373284353448));
#9794=CARTESIAN_POINT('Ctrl Pts',(0.0954058193471724,0.664062078710943,
0.760535410298491));
#9795=CARTESIAN_POINT('Ctrl Pts',(-0.317995504911745,0.680907415525936,
0.636799082423208));
#9796=CARTESIAN_POINT('Ctrl Pts',(-0.483264921611616,0.690447266925411,
0.483685722801391));
#9797=CARTESIAN_POINT('Ctrl Pts',(-0.531624460286487,0.693462936034065,
0.43149728805094));
#9798=CARTESIAN_POINT('Ctrl Pts',(-0.604845284247209,0.698696869474255,
0.330839773996165));
#9799=CARTESIAN_POINT('Ctrl Pts',(-0.703408711992183,0.709469969798145,
0.0984987021510025));
#9800=CARTESIAN_POINT('Ctrl Pts',(-0.680229358189844,0.720995021434779,
-0.198734448803209));
#9801=CARTESIAN_POINT('Ctrl Pts',(-0.534484562592715,0.733907467506484,
-0.445150691856127));
#9802=CARTESIAN_POINT('Ctrl Pts',(-0.366079777526243,0.74156757604019,-0.589608759958203));
#9803=CARTESIAN_POINT('Ctrl Pts',(-0.174590108750424,0.752554221350636,
-0.671730400299516));
#9804=CARTESIAN_POINT('Ctrl Pts',(0.0327210575797316,0.761314607562119,
-0.688577883529026));
#9805=CARTESIAN_POINT('Ctrl Pts',(0.287711988942633,0.759538617285864,-0.684617964692094));
#9806=CARTESIAN_POINT('Ctrl Pts',(0.544497969015785,0.757615772552647,-0.681818632137197));
#9807=CARTESIAN_POINT('Ctrl Pts',(0.778596989996061,0.758876900759646,-0.683695542906545));
#9808=CARTESIAN_POINT('Ctrl Pts',(1.10452217702354,0.75899378202524,-0.683855618983067));
#9809=CARTESIAN_POINT('Ctrl Pts',(1.51427783815987,0.758348873032374,-0.682909105628775));
#9810=CARTESIAN_POINT('Ctrl Pts',(1.83620533625635,0.758909242853562,-0.683725002411278));
#9811=CARTESIAN_POINT('Ctrl Pts',(2.00012854403087,0.758735125783585,-0.683469921470732));
#9812=CARTESIAN_POINT('Ctrl Pts',(0.647562717600109,-0.0686047413844538,
-2.00014688340338));
#9813=CARTESIAN_POINT('Ctrl Pts',(0.647817823654385,-0.06877887560018,-1.8362075308324));
#9814=CARTESIAN_POINT('Ctrl Pts',(0.646999311251896,-0.0682200876930409,
-1.51424075188625));
#9815=CARTESIAN_POINT('Ctrl Pts',(0.647951340387484,-0.0688620337896085,
-1.1045587808546));
#9816=CARTESIAN_POINT('Ctrl Pts',(0.647783322613642,-0.0687497485883994,
-0.778544160373208));
#9817=CARTESIAN_POINT('Ctrl Pts',(0.645922404729212,-0.0674793762396106,
-0.544360858002009));
#9818=CARTESIAN_POINT('Ctrl Pts',(0.648684014072772,-0.0694244873789363,
-0.288166569069797));
#9819=CARTESIAN_POINT('Ctrl Pts',(0.652730727559635,-0.0711516627382978,
-0.0315529265726239));
#9820=CARTESIAN_POINT('Ctrl Pts',(0.635698168786289,-0.0625351806976687,
0.170966473990833));
#9821=CARTESIAN_POINT('Ctrl Pts',(0.558803449129216,-0.0522976255106795,
0.349303642561896));
#9822=CARTESIAN_POINT('Ctrl Pts',(0.421064255675426,-0.044928704997045,
0.510662776778674));
#9823=CARTESIAN_POINT('Ctrl Pts',(0.186782551168435,-0.0327314990430446,
0.649051524597898));
#9824=CARTESIAN_POINT('Ctrl Pts',(-0.167675538339671,-0.0187626080188767,
0.67645878212063));
#9825=CARTESIAN_POINT('Ctrl Pts',(-0.574346007811733,0.000701651077454804,
0.426944282706536));
#9826=CARTESIAN_POINT('Ctrl Pts',(-0.730818163437985,0.021796163491512,
-0.0945071158682554));
#9827=CARTESIAN_POINT('Ctrl Pts',(-0.500435617268145,0.0392746662117698,
-0.478086738213446));
#9828=CARTESIAN_POINT('Ctrl Pts',(-0.178473613097707,0.0547855760479349,
-0.656278999259023));
#9829=CARTESIAN_POINT('Ctrl Pts',(0.155739197633759,0.0683907912820399,
-0.688814955739565));
#9830=CARTESIAN_POINT('Ctrl Pts',(0.530114084533772,0.0859119083272224,
-0.467609708028388));
#9831=CARTESIAN_POINT('Ctrl Pts',(0.704861976973911,0.10347820932996,-0.0700557074029037));
#9832=CARTESIAN_POINT('Ctrl Pts',(0.614140928007568,0.121079751027447,0.356150243253928));
#9833=CARTESIAN_POINT('Ctrl Pts',(0.290720381570364,0.138719347207698,0.649264750912455));
#9834=CARTESIAN_POINT('Ctrl Pts',(-0.143935197576834,0.156393884255417,
0.698027557862093));
#9835=CARTESIAN_POINT('Ctrl Pts',(-0.525695989392685,0.174102555769698,
0.483454429524658));
#9836=CARTESIAN_POINT('Ctrl Pts',(-0.71062298823528,0.191844238327655,0.0844656496154849));
#9837=CARTESIAN_POINT('Ctrl Pts',(-0.635941273898295,0.207642191616313,
-0.298078404553257));
#9838=CARTESIAN_POINT('Ctrl Pts',(-0.35655077793279,0.225441229907459,-0.624951269652307));
#9839=CARTESIAN_POINT('Ctrl Pts',(0.0868534510073472,0.243270380020131,
-0.73191354407885));
#9840=CARTESIAN_POINT('Ctrl Pts',(0.455477411176392,0.260136813586793,-0.532183195716537));
#9841=CARTESIAN_POINT('Ctrl Pts',(0.617357217331075,0.27205767557878,-0.299148538315059));
#9842=CARTESIAN_POINT('Ctrl Pts',(0.71618836382869,0.285975427384868,0.0179807600873472));
#9843=CARTESIAN_POINT('Ctrl Pts',(0.585204956240556,0.304882369925317,0.486524353131866));
#9844=CARTESIAN_POINT('Ctrl Pts',(0.0960129954608337,0.326152254444956,
0.728829046239284));
#9845=CARTESIAN_POINT('Ctrl Pts',(-0.284982589881197,0.342125765179505,
0.638272956156149));
#9846=CARTESIAN_POINT('Ctrl Pts',(-0.487146226499544,0.352782283843396,
0.485449782328244));
#9847=CARTESIAN_POINT('Ctrl Pts',(-0.639999877979491,0.363445193023275,
0.283183469426195));
#9848=CARTESIAN_POINT('Ctrl Pts',(-0.731267396964867,0.379447632097204,
-0.0985338428943742));
#9849=CARTESIAN_POINT('Ctrl Pts',(-0.487133911852248,0.400806088810658,
-0.589443413007349));
#9850=CARTESIAN_POINT('Ctrl Pts',(0.108652013139086,0.424862211386592,-0.757752991265812));
#9851=CARTESIAN_POINT('Ctrl Pts',(0.633727981828975,0.448941962928639,-0.430101733974972));
#9852=CARTESIAN_POINT('Ctrl Pts',(0.74553666345861,0.473040826939442,0.179067888189971));
#9853=CARTESIAN_POINT('Ctrl Pts',(0.369092302572918,0.497156637125847,0.672639049653024));
#9854=CARTESIAN_POINT('Ctrl Pts',(-0.179399554126267,0.518601582525948,
0.719112270123592));
#9855=CARTESIAN_POINT('Ctrl Pts',(-0.556567621013042,0.537375388258511,
0.455307243010448));
#9856=CARTESIAN_POINT('Ctrl Pts',(-0.713604967963102,0.553469940848612,
0.0942917727417075));
#9857=CARTESIAN_POINT('Ctrl Pts',(-0.665414559125122,0.566880235417034,
-0.230958493782574));
#9858=CARTESIAN_POINT('Ctrl Pts',(-0.528954541427128,0.57761190439304,-0.446644246401335));
#9859=CARTESIAN_POINT('Ctrl Pts',(-0.339076478980064,0.588342534616196,
-0.617449336631183));
#9860=CARTESIAN_POINT('Ctrl Pts',(-0.0268235233283263,0.601755594253088,
-0.718916870502273));
#9861=CARTESIAN_POINT('Ctrl Pts',(0.324255474853437,0.616509012230526,-0.633024580536174));
#9862=CARTESIAN_POINT('Ctrl Pts',(0.56499789305728,0.629918454098719,-0.41821910925962));
#9863=CARTESIAN_POINT('Ctrl Pts',(0.727572156699319,0.646008086207112,-0.0660687241023528));
#9864=CARTESIAN_POINT('Ctrl Pts',(0.629246955383781,0.666115997057895,0.440121077839912));
#9865=CARTESIAN_POINT('Ctrl Pts',(0.0963360596202998,0.690223883850523,
0.760285666107944));
#9866=CARTESIAN_POINT('Ctrl Pts',(-0.316678988048333,0.707054904105865,
0.63654207486579));
#9867=CARTESIAN_POINT('Ctrl Pts',(-0.481687401461808,0.716579782808358,
0.483670161998668));
#9868=CARTESIAN_POINT('Ctrl Pts',(-0.529964766765977,0.719590322805737,
0.431569437455635));
#9869=CARTESIAN_POINT('Ctrl Pts',(-0.603043166083147,0.724814190701037,
0.331109063559711));
#9870=CARTESIAN_POINT('Ctrl Pts',(-0.701377603074042,0.735562736341102,
0.0992698806470131));
#9871=CARTESIAN_POINT('Ctrl Pts',(-0.678208718803284,0.747052970111286,
-0.197007108721183));
#9872=CARTESIAN_POINT('Ctrl Pts',(-0.533049782551756,0.759915124360583,
-0.442527004349377));
#9873=CARTESIAN_POINT('Ctrl Pts',(-0.365130150057323,0.767553352808611,
-0.586422650312711));
#9874=CARTESIAN_POINT('Ctrl Pts',(-0.175401583891143,0.778448000940243,
-0.667878786877269));
#9875=CARTESIAN_POINT('Ctrl Pts',(0.0324402657906996,0.78723317066499,-0.684909823724877));
#9876=CARTESIAN_POINT('Ctrl Pts',(0.288015320783504,0.785452363342735,-0.680884264968639));
#9877=CARTESIAN_POINT('Ctrl Pts',(0.544474856630133,0.783531757833144,-0.678113913170131));
#9878=CARTESIAN_POINT('Ctrl Pts',(0.778496518105208,0.784792023974274,-0.679978689304889));
#9879=CARTESIAN_POINT('Ctrl Pts',(1.10461251107124,0.784909435358377,-0.680144875308017));
#9880=CARTESIAN_POINT('Ctrl Pts',(1.51420958961188,0.784264160485163,-0.679194142967422));
#9881=CARTESIAN_POINT('Ctrl Pts',(1.83620793448134,0.784824707877476,-0.680012060334172));
#9882=CARTESIAN_POINT('Ctrl Pts',(2.00015029331814,0.784650570465493,-0.679756949592654));
#9883=CARTESIAN_POINT('Ctrl Pts',(0.662463988280159,-0.0499822726657336,
-2.00015029073282));
#9884=CARTESIAN_POINT('Ctrl Pts',(0.662719098649113,-0.050156409826639,
-1.8362081654112));
#9885=CARTESIAN_POINT('Ctrl Pts',(0.661899454328382,-0.0495966927590349,
-1.51421755028528));
#9886=CARTESIAN_POINT('Ctrl Pts',(0.66284910632835,-0.0502402207575894,
-1.10458006510705));
#9887=CARTESIAN_POINT('Ctrl Pts',(0.662680367156758,-0.0501253275132676,
-0.778501033524502));
#9888=CARTESIAN_POINT('Ctrl Pts',(0.660816894629293,-0.0488599276476446,
-0.544393513999504));
#9889=CARTESIAN_POINT('Ctrl Pts',(0.663578472032617,-0.0507927293188021,
-0.288093216071113));
#9890=CARTESIAN_POINT('Ctrl Pts',(0.667616321865346,-0.05254656640794,-0.0319099260796923));
#9891=CARTESIAN_POINT('Ctrl Pts',(0.650567348477531,-0.043847011278566,
0.173143128512355));
#9892=CARTESIAN_POINT('Ctrl Pts',(0.571579298183145,-0.0333126323934734,
0.356716710686719));
#9893=CARTESIAN_POINT('Ctrl Pts',(0.430996119168082,-0.0258103364145119,
0.521087714337906));
#9894=CARTESIAN_POINT('Ctrl Pts',(0.1915071815102,-0.0133332387943894,0.662736701654699));
#9895=CARTESIAN_POINT('Ctrl Pts',(-0.170274276907979,0.000917860101533585,
0.690477633323126));
#9896=CARTESIAN_POINT('Ctrl Pts',(-0.585129454859053,0.0207803290775139,
0.435999532244355));
#9897=CARTESIAN_POINT('Ctrl Pts',(-0.744443896456613,0.0422755776723358,
-0.095507074164448));
#9898=CARTESIAN_POINT('Ctrl Pts',(-0.509841682105653,0.0600698652129145,
-0.48587284842243));
#9899=CARTESIAN_POINT('Ctrl Pts',(-0.182371420410715,0.0758462955406901,
-0.667116998551829));
#9900=CARTESIAN_POINT('Ctrl Pts',(0.157399036884807,0.0896784376807901,
-0.70013721155414));
#9901=CARTESIAN_POINT('Ctrl Pts',(0.537616507612329,0.107475858373865,-0.475407626319063));
#9902=CARTESIAN_POINT('Ctrl Pts',(0.714892343577423,0.125303248323797,-0.0719474598634416));
#9903=CARTESIAN_POINT('Ctrl Pts',(0.622850446151327,0.143150556790639,0.360164498039423));
#9904=CARTESIAN_POINT('Ctrl Pts',(0.29518893985529,0.161020474047202,0.657035729572063));
#9905=CARTESIAN_POINT('Ctrl Pts',(-0.144717629684642,0.178909688014726,
0.706323488235444));
#9906=CARTESIAN_POINT('Ctrl Pts',(-0.530705045249643,0.196817350568182,
0.489298555050095));
#9907=CARTESIAN_POINT('Ctrl Pts',(-0.717460687670318,0.214742034949024,
0.0862002289659455));
#9908=CARTESIAN_POINT('Ctrl Pts',(-0.642031232999526,0.230688899152405,
-0.29990296920214));
#9909=CARTESIAN_POINT('Ctrl Pts',(-0.360225222270616,0.248640848207253,
-0.629537751434071));
#9910=CARTESIAN_POINT('Ctrl Pts',(0.0865652378839908,0.266605936263461,
-0.737214564320495));
#9911=CARTESIAN_POINT('Ctrl Pts',(0.457579401162888,0.283585396119934,-0.536108564143753));
#9912=CARTESIAN_POINT('Ctrl Pts',(0.620386129590537,0.295575769676806,-0.301726429359565));
#9913=CARTESIAN_POINT('Ctrl Pts',(0.719733178313584,0.309567943995265,0.017099356343888));
#9914=CARTESIAN_POINT('Ctrl Pts',(0.588010276659275,0.328565400057628,0.487758585805817));
#9915=CARTESIAN_POINT('Ctrl Pts',(0.0971670852606046,0.349906037582471,
0.730730476660701));
#9916=CARTESIAN_POINT('Ctrl Pts',(-0.284652563504559,0.365915702155902,
0.639924193300074));
#9917=CARTESIAN_POINT('Ctrl Pts',(-0.487137810765924,0.376590035291017,
0.486854053066531));
#9918=CARTESIAN_POINT('Ctrl Pts',(-0.640157655994926,0.387265017474822,
0.284357621330306));
#9919=CARTESIAN_POINT('Ctrl Pts',(-0.731435491885652,0.40327851439673,-0.0976053795959151));
#9920=CARTESIAN_POINT('Ctrl Pts',(-0.487282112219958,0.424630326141765,
-0.588251513730542));
#9921=CARTESIAN_POINT('Ctrl Pts',(0.107542304304109,0.448648432219031,-0.756123031572738));
#9922=CARTESIAN_POINT('Ctrl Pts',(0.631001759798563,0.472660308219991,-0.429295319219671));
#9923=CARTESIAN_POINT('Ctrl Pts',(0.74218478195565,0.496662177151635,0.177378805470387));
#9924=CARTESIAN_POINT('Ctrl Pts',(0.367633182807851,0.520650711771743,0.668206905588921));
#9925=CARTESIAN_POINT('Ctrl Pts',(-0.177290589757161,0.541959211942665,
0.714225571639092));
#9926=CARTESIAN_POINT('Ctrl Pts',(-0.551548311632649,0.560590950253618,
0.452391321581651));
#9927=CARTESIAN_POINT('Ctrl Pts',(-0.707222318657316,0.576550987095786,
0.0943897454653029));
#9928=CARTESIAN_POINT('Ctrl Pts',(-0.659429314778723,0.589841843320291,
-0.227905593604475));
#9929=CARTESIAN_POINT('Ctrl Pts',(-0.524302856027198,0.600468553416982,
-0.441469891084629));
#9930=CARTESIAN_POINT('Ctrl Pts',(-0.336344999478411,0.611091037993889,
-0.610532913980466));
#9931=CARTESIAN_POINT('Ctrl Pts',(-0.027435641532116,0.62436110450958,-0.710885116678141));
#9932=CARTESIAN_POINT('Ctrl Pts',(0.319584613456734,0.638945190751432,-0.625937595350502));
#9933=CARTESIAN_POINT('Ctrl Pts',(0.557385963976335,0.652193001743414,-0.413741983631198));
#9934=CARTESIAN_POINT('Ctrl Pts',(0.717866358113644,0.668077414553885,-0.0660827982863029));
#9935=CARTESIAN_POINT('Ctrl Pts',(0.620756152430939,0.687913874031373,0.433187274501453));
#9936=CARTESIAN_POINT('Ctrl Pts',(0.095640770400992,0.711668836897727,0.74852107598595));
#9937=CARTESIAN_POINT('Ctrl Pts',(-0.310834112497513,0.72823701458646,0.626633342288499));
#9938=CARTESIAN_POINT('Ctrl Pts',(-0.473100780452007,0.737604098016007,
0.476301824795464));
#9939=CARTESIAN_POINT('Ctrl Pts',(-0.520571911912829,0.740564126634636,
0.42507429163648));
#9940=CARTESIAN_POINT('Ctrl Pts',(-0.592417282988213,0.745701681582158,
0.326282155767353));
#9941=CARTESIAN_POINT('Ctrl Pts',(-0.689117006009886,0.756262723952014,
0.0984423004980192));
#9942=CARTESIAN_POINT('Ctrl Pts',(-0.666140421673785,0.76756456855443,-0.192756292142937));
#9943=CARTESIAN_POINT('Ctrl Pts',(-0.523895647667715,0.780175707607948,
-0.433635461326377));
#9944=CARTESIAN_POINT('Ctrl Pts',(-0.358640415083758,0.787697519295988,
-0.575013532729149));
#9945=CARTESIAN_POINT('Ctrl Pts',(-0.173686618063833,0.798322615376446,
-0.654575062224357));
#9946=CARTESIAN_POINT('Ctrl Pts',(0.0320410938202948,0.807040382619809,
-0.671633206639044));
#9947=CARTESIAN_POINT('Ctrl Pts',(0.288083260014899,0.805282774523917,-0.667600711484946));
#9948=CARTESIAN_POINT('Ctrl Pts',(0.544416813021393,0.803352493165594,-0.664841874904024));
#9949=CARTESIAN_POINT('Ctrl Pts',(0.778500733721097,0.804617356522799,-0.666707630946455));
#9950=CARTESIAN_POINT('Ctrl Pts',(1.10459149410625,0.804732922624886,-0.666877921514692));
#9951=CARTESIAN_POINT('Ctrl Pts',(1.51421516428224,0.804089532801427,-0.665931138084407));
#9952=CARTESIAN_POINT('Ctrl Pts',(1.83620821687538,0.804649660698633,-0.66675251787415));
#9953=CARTESIAN_POINT('Ctrl Pts',(2.00015071794412,0.804475523135573,-0.666497406911305));
#9954=CARTESIAN_POINT('',(2.00009323767342,0.735984691360175,-0.676310263121555));
#9955=CARTESIAN_POINT('Origin',(1.99999999999998,0.759999999999999,-0.60000000000007));
#9956=CARTESIAN_POINT('',(0.600124355483127,-0.0799998580128369,-2.00008516830249));
#9957=CARTESIAN_POINT('Ctrl Pts',(0.600124355483126,-0.0799998580128369,
-2.00008516830249));
#9958=CARTESIAN_POINT('Ctrl Pts',(0.600379376695518,-0.0801739343158842,
-1.83620033785433));
#9959=CARTESIAN_POINT('Ctrl Pts',(0.599562611053881,-0.0796184124528264,
-1.5144754520526));
#9960=CARTESIAN_POINT('Ctrl Pts',(0.600502518404447,-0.0802525034314073,
-1.10424411057565));
#9961=CARTESIAN_POINT('Ctrl Pts',(0.600344602427935,-0.0801506833161176,
-0.778901942331774));
#9962=CARTESIAN_POINT('Ctrl Pts',(0.598456953704134,-0.0788587712934794,
-0.544242160533997));
#9963=CARTESIAN_POINT('Ctrl Pts',(0.601272474507003,-0.0808543685860998,
-0.287680267082095));
#9964=CARTESIAN_POINT('Ctrl Pts',(0.605184477979747,-0.0824681761820383,
-0.0307556431383126));
#9965=CARTESIAN_POINT('Ctrl Pts',(0.588609512632607,-0.0742202560328195,
0.161001223625551));
#9966=CARTESIAN_POINT('Ctrl Pts',(0.518063450209372,-0.0648906358873938,
0.323627369018429));
#9967=CARTESIAN_POINT('Ctrl Pts',(0.389740128736442,-0.0579722786893707,
0.474748184678881));
#9968=CARTESIAN_POINT('Ctrl Pts',(0.173020606908044,-0.0467144436845919,
0.602178110487582));
#9969=CARTESIAN_POINT('Ctrl Pts',(-0.156647509262585,-0.0336993466160229,
0.628366170043479));
#9970=CARTESIAN_POINT('Ctrl Pts',(-0.534302969503257,-0.01563383198389,
0.396152535345114));
#9971=CARTESIAN_POINT('Ctrl Pts',(-0.680181221263981,0.00400588873282267,
-0.0887030397692518));
#9972=CARTESIAN_POINT('Ctrl Pts',(-0.465603142330848,0.0202821362637637,
-0.446134214125788));
#9973=CARTESIAN_POINT('Ctrl Pts',(-0.165486932860075,0.03474270768116,-0.612245575240685));
#9974=CARTESIAN_POINT('Ctrl Pts',(0.146295095787791,0.0474352484480225,
-0.642641412885972));
#9975=CARTESIAN_POINT('Ctrl Pts',(0.495949774692522,0.0637997238881112,
-0.436123139243827));
#9976=CARTESIAN_POINT('Ctrl Pts',(0.659385538859151,0.0802233041204479,
-0.0644782106763051));
#9977=CARTESIAN_POINT('Ctrl Pts',(0.574545201045043,0.0966991572901908,
0.334449484668907));
#9978=CARTESIAN_POINT('Ctrl Pts',(0.271532605139402,0.113229721085999,0.609171048717871));
#9979=CARTESIAN_POINT('Ctrl Pts',(-0.136251969463658,0.129813195665052,
0.654997123118035));
#9980=CARTESIAN_POINT('Ctrl Pts',(-0.494901592911036,0.146449576154649,
0.453502429895765));
#9981=CARTESIAN_POINT('Ctrl Pts',(-0.668917284177339,0.163138203343486,
0.0782620703516101));
#9982=CARTESIAN_POINT('Ctrl Pts',(-0.598644996586867,0.178018517289954,
-0.282046799603755));
#9983=CARTESIAN_POINT('Ctrl Pts',(-0.335262243900907,0.194801447000121,
-0.590258574308657));
#9984=CARTESIAN_POINT('Ctrl Pts',(0.0833281156314849,0.211635077569448,
-0.691395156339746));
#9985=CARTESIAN_POINT('Ctrl Pts',(0.4320119853653,0.227588446215705,-0.502587368796631));
#9986=CARTESIAN_POINT('Ctrl Pts',(0.58527223262087,0.238874211068699,-0.281979562605746));
#9987=CARTESIAN_POINT('Ctrl Pts',(0.678917739338141,0.252059849462334,0.0184388692246381));
#9988=CARTESIAN_POINT('Ctrl Pts',(0.554821413577227,0.270001502682695,0.463024783480917));
#9989=CARTESIAN_POINT('Ctrl Pts',(0.089888824047859,0.290221470828933,0.693551038003489));
#9990=CARTESIAN_POINT('Ctrl Pts',(-0.272915151999609,0.305432097922516,
0.607393400489082));
#9991=CARTESIAN_POINT('Ctrl Pts',(-0.465626168527264,0.315590515005467,
0.46173311346713));
#9992=CARTESIAN_POINT('Ctrl Pts',(-0.611423927492396,0.325760833794014,
0.268821318511434));
#9993=CARTESIAN_POINT('Ctrl Pts',(-0.698650473779508,0.341042831595186,
-0.0956472554953462));
#9994=CARTESIAN_POINT('Ctrl Pts',(-0.465321982498693,0.361476665326508,
-0.565350807747607));
#9995=CARTESIAN_POINT('Ctrl Pts',(0.10575120321005,0.38454069790763,-0.726974188805798));
#9996=CARTESIAN_POINT('Ctrl Pts',(0.610387251745808,0.407678360873112,-0.412408779209339));
#9997=CARTESIAN_POINT('Ctrl Pts',(0.718323895495084,0.430887045922702,0.17413060542287));
#9998=CARTESIAN_POINT('Ctrl Pts',(0.355237119019683,0.454164351458316,0.650683811024646));
#9999=CARTESIAN_POINT('Ctrl Pts',(-0.175382406590221,0.4749142230429,0.695878649309196));
#10000=CARTESIAN_POINT('Ctrl Pts',(-0.54101475967607,0.49311138275633,0.440269492223299));
#10001=CARTESIAN_POINT('Ctrl Pts',(-0.693527526572458,0.50873629806685,
0.0898379898580044));
#10002=CARTESIAN_POINT('Ctrl Pts',(-0.646735970560938,0.521779183073869,
-0.226461651899009));
#10003=CARTESIAN_POINT('Ctrl Pts',(-0.513906112786406,0.532226370805735,
-0.436433419735239));
#10004=CARTESIAN_POINT('Ctrl Pts',(-0.328920782360512,0.542681936352062,
-0.602852159734885));
#10005=CARTESIAN_POINT('Ctrl Pts',(-0.0243494995865983,0.55576702001899,
-0.701905622444322));
#10006=CARTESIAN_POINT('Ctrl Pts',(0.318684360355662,0.570182439320145,
-0.618057422392217));
#10007=CARTESIAN_POINT('Ctrl Pts',(0.554275268889935,0.583304705413154,
-0.407908493988256));
#10008=CARTESIAN_POINT('Ctrl Pts',(0.713586310862138,0.599067032359038,
-0.0629718800249659));
#10009=CARTESIAN_POINT('Ctrl Pts',(0.617323759198901,0.61880473745743,0.433855029903579));
#10010=CARTESIAN_POINT('Ctrl Pts',(0.0931818027763926,0.642526983889894,
0.749181117386836));
#10011=CARTESIAN_POINT('Ctrl Pts',(-0.314313763037281,0.659133011706964,
0.627311226200405));
#10012=CARTESIAN_POINT('Ctrl Pts',(-0.477269723836412,0.668539639010893,
0.476341934975343));
#10013=CARTESIAN_POINT('Ctrl Pts',(-0.524957853949116,0.671513213020625,
0.424882768662061));
#10014=CARTESIAN_POINT('Ctrl Pts',(-0.597179322807005,0.676677358782867,
0.325569816011966));
#10015=CARTESIAN_POINT('Ctrl Pts',(-0.69448376569806,0.6873032670482,0.0964041117283874));
#10016=CARTESIAN_POINT('Ctrl Pts',(-0.671478747098358,0.69869719950028,
-0.197322255866813));
#10017=CARTESIAN_POINT('Ctrl Pts',(-0.527686488423399,0.711441182605667,
-0.440569074748579));
#10018=CARTESIAN_POINT('Ctrl Pts',(-0.36114955668007,0.719020822056164,
-0.583433135906584));
#10019=CARTESIAN_POINT('Ctrl Pts',(-0.171544666302877,0.729888896055897,
-0.664752607658936));
#10020=CARTESIAN_POINT('Ctrl Pts',(0.0327819626725445,0.738541246775484,
-0.681326463162123));
#10021=CARTESIAN_POINT('Ctrl Pts',(0.287281763425397,0.736796378226309,
-0.677467579294977));
#10022=CARTESIAN_POINT('Ctrl Pts',(0.544477498698488,0.734860197456536,
-0.674632411152923));
#10023=CARTESIAN_POINT('Ctrl Pts',(0.778765801010588,0.736127346477361,
-0.676530344298986));
#10024=CARTESIAN_POINT('Ctrl Pts',(1.10435275137728,0.736241519844584,-0.676684603908725));
#10025=CARTESIAN_POINT('Ctrl Pts',(1.51439530422594,0.735599108498541,-0.675749139626198));
#10026=CARTESIAN_POINT('Ctrl Pts',(1.83620130898864,0.736158775205915,-0.676565295388702));
#10027=CARTESIAN_POINT('Ctrl Pts',(2.00009323767342,0.735984691360175,-0.676310263121555));
#10028=CARTESIAN_POINT('Origin',(0.6,0.,-2.));
#10029=CARTESIAN_POINT('Ctrl Pts',(0.528325516000818,0.0355351383793534,
-1.99985072236852));
#10030=CARTESIAN_POINT('Ctrl Pts',(0.528580216238454,0.0353612811721935,
-1.83617216061816));
#10031=CARTESIAN_POINT('Ctrl Pts',(0.527763128960968,0.0359074110765236,
-1.51524836790432));
#10032=CARTESIAN_POINT('Ctrl Pts',(0.52869398879819,0.0352930571869228,
-1.10323975855771));
#10033=CARTESIAN_POINT('Ctrl Pts',(0.528539994622404,0.0353667487690795,
-0.780063536259368));
#10034=CARTESIAN_POINT('Ctrl Pts',(0.52663921660727,0.0367139095688948,
-0.544390644686365));
#10035=CARTESIAN_POINT('Ctrl Pts',(0.529476659613029,0.034585865490992,
-0.284703947187213));
#10036=CARTESIAN_POINT('Ctrl Pts',(0.533317427829506,0.0332656496173089,
-0.0318821597569514));
#10037=CARTESIAN_POINT('Ctrl Pts',(0.520047835906791,0.03934019911185,0.11127177591819));
#10038=CARTESIAN_POINT('Ctrl Pts',(0.487979861380134,0.0447394305988247,
0.206368682333952));
#10039=CARTESIAN_POINT('Ctrl Pts',(0.43700205055529,0.0496761629927893,
0.303336604975879));
#10040=CARTESIAN_POINT('Ctrl Pts',(0.343595116172016,0.0549025285724336,
0.412156142305733));
#10041=CARTESIAN_POINT('Ctrl Pts',(0.155413324632073,0.0645663572156617,
0.523171635285862));
#10042=CARTESIAN_POINT('Ctrl Pts',(-0.13238197811405,0.0760053922841299,
0.546096961811003));
#10043=CARTESIAN_POINT('Ctrl Pts',(-0.458547546709041,0.0915759716479705,
0.344626269173423));
#10044=CARTESIAN_POINT('Ctrl Pts',(-0.583900979357653,0.108513502601817,
-0.0726418166757439));
#10045=CARTESIAN_POINT('Ctrl Pts',(-0.399874479395914,0.122418645633365,
-0.378151431589044));
#10046=CARTESIAN_POINT('Ctrl Pts',(-0.144208713332262,0.134741070398731,
-0.519625470017589));
#10047=CARTESIAN_POINT('Ctrl Pts',(0.120678163831248,0.145520914168386,
-0.545280477556419));
#10048=CARTESIAN_POINT('Ctrl Pts',(0.416245026241475,0.159362036169617,
-0.370399044184566));
#10049=CARTESIAN_POINT('Ctrl Pts',(0.553682940345137,0.173192726374506,
-0.0573370873951302));
#10050=CARTESIAN_POINT('Ctrl Pts',(0.482308934415198,0.187011877340453,
0.277215748417183));
#10051=CARTESIAN_POINT('Ctrl Pts',(0.229028777221665,0.200821622625116,
0.506563345532159));
#10052=CARTESIAN_POINT('Ctrl Pts',(-0.110367911292249,0.214623077889557,
0.54450512639393));
#10053=CARTESIAN_POINT('Ctrl Pts',(-0.407671943899019,0.228418134002614,
0.377255910602494));
#10054=CARTESIAN_POINT('Ctrl Pts',(-0.551281224571261,0.242207799546803,
0.0671237295171103));
#10055=CARTESIAN_POINT('Ctrl Pts',(-0.493275743670343,0.254462041472817,
-0.229567370520871));
#10056=CARTESIAN_POINT('Ctrl Pts',(-0.276873119070605,0.268246207770326,
-0.482655650599567));
#10057=CARTESIAN_POINT('Ctrl Pts',(0.0659203358970661,0.282029146223394,
-0.565205026128377));
#10058=CARTESIAN_POINT('Ctrl Pts',(0.350357710654226,0.295047091504507,
-0.410999506466758));
#10059=CARTESIAN_POINT('Ctrl Pts',(0.475135516148999,0.304237345274322,
-0.231346154144024));
#10060=CARTESIAN_POINT('Ctrl Pts',(0.551288205940918,0.314960561464671,
0.0129747269886634));
#10061=CARTESIAN_POINT('Ctrl Pts',(0.45022254899038,0.329517029083473,0.37370896603078));
#10062=CARTESIAN_POINT('Ctrl Pts',(0.0742959024516958,0.345869925490746,
0.559751696715401));
#10063=CARTESIAN_POINT('Ctrl Pts',(-0.267515912073187,0.360187665470484,
0.478838803845945));
#10064=CARTESIAN_POINT('Ctrl Pts',(-0.479551721793889,0.372466952348416,
0.266530966916759));
#10065=CARTESIAN_POINT('Ctrl Pts',(-0.561020874450445,0.386802304141767,
-0.0756540266283994));
#10066=CARTESIAN_POINT('Ctrl Pts',(-0.373798964410677,0.40320076690853,
-0.452338944214845));
#10067=CARTESIAN_POINT('Ctrl Pts',(0.0837095501434262,0.421672873429502,
-0.581681018186793));
#10068=CARTESIAN_POINT('Ctrl Pts',(0.487056597627596,0.440172228021392,
-0.33000386321063));
#10069=CARTESIAN_POINT('Ctrl Pts',(0.573129832954481,0.458702467353384,
0.138301209287518));
#10070=CARTESIAN_POINT('Ctrl Pts',(0.283467753989205,0.477266746895905,
0.518306234712299));
#10071=CARTESIAN_POINT('Ctrl Pts',(-0.139343171325179,0.49380124199818,
0.554254940466149));
#10072=CARTESIAN_POINT('Ctrl Pts',(-0.430585233273848,0.508295268221301,
0.350657311113887));
#10073=CARTESIAN_POINT('Ctrl Pts',(-0.551985372269875,0.520737714298862,
0.0715900336355947));
#10074=CARTESIAN_POINT('Ctrl Pts',(-0.507419925273811,0.533200036247129,
-0.230607774684784));
#10075=CARTESIAN_POINT('Ctrl Pts',(-0.31033354343041,0.545683195018118,
-0.464206836172492));
#10076=CARTESIAN_POINT('Ctrl Pts',(-0.0190318124706425,0.55818804173365,
-0.558876538153605));
#10077=CARTESIAN_POINT('Ctrl Pts',(0.253983768099081,0.569671725898546,
-0.492060874631647));
#10078=CARTESIAN_POINT('Ctrl Pts',(0.442244523118364,0.580128296331906,
-0.324658610947337));
#10079=CARTESIAN_POINT('Ctrl Pts',(0.520722105088888,0.587982684618036,
-0.152670499369794));
#10080=CARTESIAN_POINT('Ctrl Pts',(0.546710027901627,0.597417021784907,
0.0692065446470551));
#10081=CARTESIAN_POINT('Ctrl Pts',(0.456423583474616,0.610019390825592,
0.367751194847143));
#10082=CARTESIAN_POINT('Ctrl Pts',(0.0741878943616268,0.627382577648326,
0.598649005107442));
#10083=CARTESIAN_POINT('Ctrl Pts',(-0.252446137124855,0.640668092490499,
0.501260226779611));
#10084=CARTESIAN_POINT('Ctrl Pts',(-0.382734909615739,0.648193686386572,
0.380473706897257));
#10085=CARTESIAN_POINT('Ctrl Pts',(-0.42091088190008,0.650570748345437,
0.339327536657439));
#10086=CARTESIAN_POINT('Ctrl Pts',(-0.478799050747207,0.654727247608708,
0.259486984260798));
#10087=CARTESIAN_POINT('Ctrl Pts',(-0.557131063499655,0.663174776823465,
0.0765261952556552));
#10088=CARTESIAN_POINT('Ctrl Pts',(-0.537566049825482,0.672499456879064,
-0.160776378174217));
#10089=CARTESIAN_POINT('Ctrl Pts',(-0.423528711452778,0.682478562361745,
-0.354330430488681));
#10090=CARTESIAN_POINT('Ctrl Pts',(-0.311592387005274,0.687842301956471,
-0.450400927405352));
#10091=CARTESIAN_POINT('Ctrl Pts',(-0.211665405946688,0.692933513783124,
-0.502993006931043));
#10092=CARTESIAN_POINT('Ctrl Pts',(-0.112852189303309,0.69854100703458,
-0.536239978733061));
#10093=CARTESIAN_POINT('Ctrl Pts',(0.0321928148234355,0.704663557813275,
-0.549477537118094));
#10094=CARTESIAN_POINT('Ctrl Pts',(0.28467574209202,0.703327852119614,-0.545661762520716));
#10095=CARTESIAN_POINT('Ctrl Pts',(0.544418006349421,0.701207276752475,
-0.542811541675268));
#10096=CARTESIAN_POINT('Ctrl Pts',(0.780045344880861,0.702551643433085,
-0.544716466237711));
#10097=CARTESIAN_POINT('Ctrl Pts',(1.10325708111259,0.702626966137619,-0.544867419416464));
#10098=CARTESIAN_POINT('Ctrl Pts',(1.5152368295222,0.70201184590394,-0.543937156859423));
#10099=CARTESIAN_POINT('Ctrl Pts',(1.83617236681158,0.702558621549799,-0.544752786768393));
#10100=CARTESIAN_POINT('Ctrl Pts',(1.9998524353109,0.702384762739154,-0.544498084176928));
#10101=CARTESIAN_POINT('Ctrl Pts',(0.518006988619909,0.0147226621587207,
-1.99985677244376));
#10102=CARTESIAN_POINT('Ctrl Pts',(0.51826169653407,0.0145487997116001,
-1.83617327751152));
#10103=CARTESIAN_POINT('Ctrl Pts',(0.517439258498296,0.0150951255434231,
-1.51522865062124));
#10104=CARTESIAN_POINT('Ctrl Pts',(0.518364404194574,0.0144817764415016,
-1.10324322288189));
#10105=CARTESIAN_POINT('Ctrl Pts',(0.518203712856234,0.0145552635795002,
-0.780023366489656));
#10106=CARTESIAN_POINT('Ctrl Pts',(0.516302146489189,0.0159040910419349,
-0.544343077372114));
#10107=CARTESIAN_POINT('Ctrl Pts',(0.519119939486031,0.0137739026997169,
-0.284772538321969));
#10108=CARTESIAN_POINT('Ctrl Pts',(0.522975085576804,0.0124609380717381,
-0.0315732326310645));
#10109=CARTESIAN_POINT('Ctrl Pts',(0.509643674692382,0.018517597343244,
0.110651199452232));
#10110=CARTESIAN_POINT('Ctrl Pts',(0.47832511502757,0.0237806788581772,
0.203319306803046));
#10111=CARTESIAN_POINT('Ctrl Pts',(0.428443867571616,0.028616054359568,
0.29829212926619));
#10112=CARTESIAN_POINT('Ctrl Pts',(0.336639314786772,0.033752976935528,
0.405215900979145));
#10113=CARTESIAN_POINT('Ctrl Pts',(0.151994665964955,0.0432358978067775,
0.514121724925737));
#10114=CARTESIAN_POINT('Ctrl Pts',(-0.130966602912282,0.0544866325216903,
0.536764222009815));
#10115=CARTESIAN_POINT('Ctrl Pts',(-0.451809607501558,0.0698051303173712,
0.338584434964127));
#10116=CARTESIAN_POINT('Ctrl Pts',(-0.575501058572054,0.0864976418736099,
-0.072428206504078));
#10117=CARTESIAN_POINT('Ctrl Pts',(-0.394000818625767,0.100217666459796,
-0.373861821833153));
#10118=CARTESIAN_POINT('Ctrl Pts',(-0.141611300945278,0.112384059902738,
-0.513558715621065));
#10119=CARTESIAN_POINT('Ctrl Pts',(0.120151382692751,0.123039230651802,
-0.538926981640901));
#10120=CARTESIAN_POINT('Ctrl Pts',(0.412599084171835,0.136736320530498,
-0.365982567622163));
#10121=CARTESIAN_POINT('Ctrl Pts',(0.548778764164466,0.150437544146518,
-0.0559340071012521));
#10122=CARTESIAN_POINT('Ctrl Pts',(0.478069875663281,0.164143621167663,
0.275811473392926));
#10123=CARTESIAN_POINT('Ctrl Pts',(0.226673355209394,0.177856074698083,
0.503539697370229));
#10124=CARTESIAN_POINT('Ctrl Pts',(-0.110644606215152,0.191576390642706,
0.541311737028743));
#10125=CARTESIAN_POINT('Ctrl Pts',(-0.406509930397425,0.20530665826345,
0.374938573118697));
#10126=CARTESIAN_POINT('Ctrl Pts',(-0.549639073980249,0.219047557375228,
0.0659995113422246));
#10127=CARTESIAN_POINT('Ctrl Pts',(-0.491828299868531,0.231273972126515,
-0.229959181959865));
#10128=CARTESIAN_POINT('Ctrl Pts',(-0.27580622579465,0.245037965029692,
-0.482642962691277));
#10129=CARTESIAN_POINT('Ctrl Pts',(0.0667891693692878,0.258815642204134,
-0.56526745809795));
#10130=CARTESIAN_POINT('Ctrl Pts',(0.351583495751141,0.271851711458274,
-0.41095497024062));
#10131=CARTESIAN_POINT('Ctrl Pts',(0.476585714824317,0.281058974417471,
-0.230992328401952));
#10132=CARTESIAN_POINT('Ctrl Pts',(0.552929626102851,0.291807850647884,
0.0138816394099051));
#10133=CARTESIAN_POINT('Ctrl Pts',(0.451593915839779,0.306425020358756,
0.375986515342406));
#10134=CARTESIAN_POINT('Ctrl Pts',(0.0738204095193084,0.322862572045568,
0.563103116958926));
#10135=CARTESIAN_POINT('Ctrl Pts',(-0.270167738435555,0.337272921272754,
0.481717326921321));
#10136=CARTESIAN_POINT('Ctrl Pts',(-0.483806774332006,0.349644528947839,
0.267882725040153));
#10137=CARTESIAN_POINT('Ctrl Pts',(-0.56600730933755,0.364102175236501,
-0.0771625257846216));
#10138=CARTESIAN_POINT('Ctrl Pts',(-0.377092271910289,0.380665601055743,
-0.457594185300374));
#10139=CARTESIAN_POINT('Ctrl Pts',(0.0855089279844419,0.399348369251059,
-0.588538803959294));
#10140=CARTESIAN_POINT('Ctrl Pts',(0.494066616980439,0.418086689130485,
-0.333792905023513));
#10141=CARTESIAN_POINT('Ctrl Pts',(0.581499054249072,0.436883611950722,
0.1411231143738));
#10142=CARTESIAN_POINT('Ctrl Pts',(0.287433008810201,0.455740676787563,
0.527163124276987));
#10143=CARTESIAN_POINT('Ctrl Pts',(-0.142615978537236,0.47256294829645,
0.563831621580814));
#10144=CARTESIAN_POINT('Ctrl Pts',(-0.439170122070614,0.487320513166624,
0.356588512723425));
#10145=CARTESIAN_POINT('Ctrl Pts',(-0.562904282860289,0.500001367061856,
0.0722157106208628));
#10146=CARTESIAN_POINT('Ctrl Pts',(-0.517490882361781,0.512715724688964,
-0.236051271509166));
#10147=CARTESIAN_POINT('Ctrl Pts',(-0.316295712666788,0.5254626426108,-0.474559379294206));
#10148=CARTESIAN_POINT('Ctrl Pts',(-0.0186872380461836,0.538239998427524,
-0.571332456617058));
#10149=CARTESIAN_POINT('Ctrl Pts',(0.260497964274366,0.549984096113616,
-0.503029943852036));
#10150=CARTESIAN_POINT('Ctrl Pts',(0.453172437169254,0.560685984855627,
-0.331743989022342));
#10151=CARTESIAN_POINT('Ctrl Pts',(0.533542764846318,0.568729832734574,
-0.155636638327312));
#10152=CARTESIAN_POINT('Ctrl Pts',(0.56017130075111,0.578393043619417,0.0716182619860427));
#10153=CARTESIAN_POINT('Ctrl Pts',(0.467665246161068,0.591312818479437,
0.377633597364541));
#10154=CARTESIAN_POINT('Ctrl Pts',(0.0755416097489565,0.609130487126725,
0.614648364140295));
#10155=CARTESIAN_POINT('Ctrl Pts',(-0.25999452114002,0.622779933154743,
0.514691601607703));
#10156=CARTESIAN_POINT('Ctrl Pts',(-0.393897285477323,0.630514235023044,
0.390563383963501));
#10157=CARTESIAN_POINT('Ctrl Pts',(-0.433131000099862,0.632957419536418,
0.34827185345534));
#10158=CARTESIAN_POINT('Ctrl Pts',(-0.492626078021695,0.637228232855216,
0.266240605920182));
#10159=CARTESIAN_POINT('Ctrl Pts',(-0.573128984843918,0.64591806968787,
0.0780451747198588));
#10160=CARTESIAN_POINT('Ctrl Pts',(-0.553160666421587,0.655505290269903,
-0.165943772968861));
#10161=CARTESIAN_POINT('Ctrl Pts',(-0.43559455019087,0.665789433238246,
-0.365425437099108));
#10162=CARTESIAN_POINT('Ctrl Pts',(-0.320468157151283,0.671307222232064,
-0.464218402012083));
#10163=CARTESIAN_POINT('Ctrl Pts',(-0.217516188562935,0.676551531702204,
-0.518462754427448));
#10164=CARTESIAN_POINT('Ctrl Pts',(-0.114896708172773,0.682375360770741,
-0.552926885225282));
#10165=CARTESIAN_POINT('Ctrl Pts',(0.0324089213706158,0.68855646510286,
-0.566177806035642));
#10166=CARTESIAN_POINT('Ctrl Pts',(0.284694547996705,0.68720379020063,-0.562380851818847));
#10167=CARTESIAN_POINT('Ctrl Pts',(0.544416635062839,0.685091793638103,
-0.559529116763886));
#10168=CARTESIAN_POINT('Ctrl Pts',(0.779973909884199,0.686433174919341,
-0.561439259023152));
#10169=CARTESIAN_POINT('Ctrl Pts',(1.10328957662273,0.686510451152178,-0.561591177867606));
#10170=CARTESIAN_POINT('Ctrl Pts',(1.51519744302046,0.685894630299126,-0.560665320718706));
#10171=CARTESIAN_POINT('Ctrl Pts',(1.83617381496558,0.686442247831574,-0.561482812535836));
#10172=CARTESIAN_POINT('Ctrl Pts',(1.99986135028159,0.686268381089775,-0.561228098325256));
#10173=CARTESIAN_POINT('Ctrl Pts',(0.517064965384546,-0.0276174348744286,
-1.99990027965328));
#10174=CARTESIAN_POINT('Ctrl Pts',(0.517319733648456,-0.0277913385160093,
-1.83617800203207));
#10175=CARTESIAN_POINT('Ctrl Pts',(0.516501154978697,-0.0272448942899652,
-1.51509441856937));
#10176=CARTESIAN_POINT('Ctrl Pts',(0.517439825994783,-0.0278604744543955,
-1.10345697185989));
#10177=CARTESIAN_POINT('Ctrl Pts',(0.51727868303505,-0.0277855206568046,
-0.779843367061392));
#10178=CARTESIAN_POINT('Ctrl Pts',(0.515395748265278,-0.0264409292158762,
-0.544362732023317));
#10179=CARTESIAN_POINT('Ctrl Pts',(0.518196318364542,-0.0285631971806174,
-0.285399374400077));
#10180=CARTESIAN_POINT('Ctrl Pts',(0.522130009157292,-0.0298969535989713,
-0.0312837912576946));
#10181=CARTESIAN_POINT('Ctrl Pts',(0.508630669142978,-0.0237744096040658,
0.11273833187974));
#10182=CARTESIAN_POINT('Ctrl Pts',(0.477303002332513,-0.0185175895096401,
0.205186241209719));
#10183=CARTESIAN_POINT('Ctrl Pts',(0.42771780622717,-0.0137076224884299,
0.299712541386803));
#10184=CARTESIAN_POINT('Ctrl Pts',(0.335710255161657,-0.00855651946997313,
0.406906376567326));
#10185=CARTESIAN_POINT('Ctrl Pts',(0.150598154466753,0.000948902484060557,
0.516127151823611));
#10186=CARTESIAN_POINT('Ctrl Pts',(-0.133196632035283,0.0122299278698042,
0.538860692452965));
#10187=CARTESIAN_POINT('Ctrl Pts',(-0.456043768540289,0.0276354505277528,
0.339704505103172));
#10188=CARTESIAN_POINT('Ctrl Pts',(-0.580879226861971,0.0444564053811016,
-0.0746224708782053));
#10189=CARTESIAN_POINT('Ctrl Pts',(-0.397598943967096,0.0583258466825628,
-0.379524117797193));
#10190=CARTESIAN_POINT('Ctrl Pts',(-0.141860962022226,0.0706512785723848,
-0.52105662949048));
#10191=CARTESIAN_POINT('Ctrl Pts',(0.123618324751229,0.0814558379837331,
-0.546900551930632));
#10192=CARTESIAN_POINT('Ctrl Pts',(0.420944460563251,0.0953736393877776,
-0.371199562504824));
#10193=CARTESIAN_POINT('Ctrl Pts',(0.55975828999923,0.10932616565685,-0.0554275481068647));
#10194=CARTESIAN_POINT('Ctrl Pts',(0.487690702846842,0.123311797342578,
0.283210359890105));
#10195=CARTESIAN_POINT('Ctrl Pts',(0.230638240284097,0.137332741277447,
0.516210623580482));
#10196=CARTESIAN_POINT('Ctrl Pts',(-0.115050726500188,0.151389888098985,
0.555028062340877));
#10197=CARTESIAN_POINT('Ctrl Pts',(-0.418919310186353,0.165484870541764,
0.384283721259028));
#10198=CARTESIAN_POINT('Ctrl Pts',(-0.566287603572425,0.179618646099089,
0.0664636290862337));
#10199=CARTESIAN_POINT('Ctrl Pts',(-0.506778045012059,0.192217438048822,
-0.238621244470182));
#10200=CARTESIAN_POINT('Ctrl Pts',(-0.283781109838095,0.206426241219143,
-0.49957208381572));
#10201=CARTESIAN_POINT('Ctrl Pts',(0.0706066034421951,0.220677604075878,
-0.585193411698452));
#10202=CARTESIAN_POINT('Ctrl Pts',(0.365832693978764,0.234183813926373,
-0.42534652150558));
#10203=CARTESIAN_POINT('Ctrl Pts',(0.495619738153408,0.243741154450391,
-0.238511686590906));
#10204=CARTESIAN_POINT('Ctrl Pts',(0.57495990921569,0.254909247382493,0.0159208359312727));
#10205=CARTESIAN_POINT('Ctrl Pts',(0.469740551468291,0.270107361335315,
0.392695173251977));
#10206=CARTESIAN_POINT('Ctrl Pts',(0.0757962012645511,0.287249204171579,
0.588020269692376));
#10207=CARTESIAN_POINT('Ctrl Pts',(-0.283683402920196,0.302304485175122,
0.503073075011702));
#10208=CARTESIAN_POINT('Ctrl Pts',(-0.507263064087155,0.315247977872081,
0.279334514400664));
#10209=CARTESIAN_POINT('Ctrl Pts',(-0.593480268797605,0.330395219740859,
-0.0821951824371391));
#10210=CARTESIAN_POINT('Ctrl Pts',(-0.395345834233177,0.34777246937306,
-0.481527416128932));
#10211=CARTESIAN_POINT('Ctrl Pts',(0.091088459307557,0.367415692906852,
-0.619429636770056));
#10212=CARTESIAN_POINT('Ctrl Pts',(0.521654838632725,0.387153663215753,
-0.351178853221841));
#10213=CARTESIAN_POINT('Ctrl Pts',(0.614127000564708,0.406988410964741,
0.150060798600657));
#10214=CARTESIAN_POINT('Ctrl Pts',(0.303351339173566,0.426921933914876,
0.558318532423771));
#10215=CARTESIAN_POINT('Ctrl Pts',(-0.15200412641022,0.444728306814291,
0.597312366353538));
#10216=CARTESIAN_POINT('Ctrl Pts',(-0.46651007651178,0.460376324275656,
0.377578786974955));
#10217=CARTESIAN_POINT('Ctrl Pts',(-0.597896215312271,0.473834148081358,
0.0757644518309022));
#10218=CARTESIAN_POINT('Ctrl Pts',(-0.549688991211359,0.487337171079593,
-0.251696035827126));
#10219=CARTESIAN_POINT('Ctrl Pts',(-0.33582481262013,0.500886334893807,
-0.505310469715122));
#10220=CARTESIAN_POINT('Ctrl Pts',(-0.0191083072298206,0.51448271913657,
-0.608315954390084));
#10221=CARTESIAN_POINT('Ctrl Pts',(0.278244251614214,0.526989032687595,
-0.535616391608276));
#10222=CARTESIAN_POINT('Ctrl Pts',(0.483576818183559,0.538392269039443,
-0.353074191952224));
#10223=CARTESIAN_POINT('Ctrl Pts',(0.569283164476684,0.546967375765335,
-0.1653038864453));
#10224=CARTESIAN_POINT('Ctrl Pts',(0.597681099378553,0.557277057685444,
0.0771548913991258));
#10225=CARTESIAN_POINT('Ctrl Pts',(0.499022954209422,0.571061850450283,
0.403754875104057));
#10226=CARTESIAN_POINT('Ctrl Pts',(0.0801878602785286,0.59009117728441,
0.656954926766208));
#10227=CARTESIAN_POINT('Ctrl Pts',(-0.278435050767254,0.604675594610773,
0.550184775122633));
#10228=CARTESIAN_POINT('Ctrl Pts',(-0.421702877060122,0.612949989901589,
0.417381582961095));
#10229=CARTESIAN_POINT('Ctrl Pts',(-0.463678194708879,0.615564544680876,
0.372121041656761));
#10230=CARTESIAN_POINT('Ctrl Pts',(-0.527311587821278,0.62012833630386,
0.284465723612475));
#10231=CARTESIAN_POINT('Ctrl Pts',(-0.613338062910082,0.62943639172353,
0.0828777024836109));
#10232=CARTESIAN_POINT('Ctrl Pts',(-0.592374455216482,0.639666807274975,
-0.177632373915939));
#10233=CARTESIAN_POINT('Ctrl Pts',(-0.465998063899403,0.650709650428148,
-0.391877889696578));
#10234=CARTESIAN_POINT('Ctrl Pts',(-0.342932122259441,0.656609679460992,
-0.497401597437851));
#10235=CARTESIAN_POINT('Ctrl Pts',(-0.232874147112921,0.662211754394164,
-0.555492407774234));
#10236=CARTESIAN_POINT('Ctrl Pts',(-0.121097630640796,0.668559783851406,
-0.592927928496883));
#10237=CARTESIAN_POINT('Ctrl Pts',(0.0328311030844529,0.674923577641489,
-0.606297423549468));
#10238=CARTESIAN_POINT('Ctrl Pts',(0.285189029776664,0.673515276722222,
-0.602484355047046));
#10239=CARTESIAN_POINT('Ctrl Pts',(0.544464931121522,0.671428302466708,
-0.599629698570021));
#10240=CARTESIAN_POINT('Ctrl Pts',(0.779716204754393,0.672759167364569,
-0.601534551529286));
#10241=CARTESIAN_POINT('Ctrl Pts',(1.10352456500245,0.672841678894774,-0.60168402557845));
#10242=CARTESIAN_POINT('Ctrl Pts',(1.51502500132075,0.67222198428823,-0.600751926240327));
#10243=CARTESIAN_POINT('Ctrl Pts',(1.83617907898506,0.672771254551909,-0.601566211172317));
#10244=CARTESIAN_POINT('Ctrl Pts',(1.99990920276725,0.672597342573202,-0.601311430689815));
#10245=CARTESIAN_POINT('Ctrl Pts',(0.553753009580757,-0.0708264141617583,
-2.00000326593235));
#10246=CARTESIAN_POINT('Ctrl Pts',(0.554007918554055,-0.0710004138509187,
-1.83619056393385));
#10247=CARTESIAN_POINT('Ctrl Pts',(0.553185359331648,-0.0704511009669655,
-1.51473935544524));
#10248=CARTESIAN_POINT('Ctrl Pts',(0.554128520828115,-0.0710714148493772,
-1.10390624361236));
#10249=CARTESIAN_POINT('Ctrl Pts',(0.55395750433957,-0.0709884976154986,
-0.779299644098123));
#10250=CARTESIAN_POINT('Ctrl Pts',(0.552089915743917,-0.0696580104253656,
-0.544343141096708));
#10251=CARTESIAN_POINT('Ctrl Pts',(0.554847476208613,-0.0717441098715436,
-0.286553871632578));
#10252=CARTESIAN_POINT('Ctrl Pts',(0.558871807050512,-0.0731549107076979,
-0.0311242532742824));
#10253=CARTESIAN_POINT('Ctrl Pts',(0.544996993740645,-0.06677124873102,
0.121479781678294));
#10254=CARTESIAN_POINT('Ctrl Pts',(0.510876588740922,-0.0610344785127724,
0.222168271083783));
#10255=CARTESIAN_POINT('Ctrl Pts',(0.458090774579739,-0.0559238546714361,
0.32273079639211));
#10256=CARTESIAN_POINT('Ctrl Pts',(0.359454280516197,-0.0503913533949749,
0.437723219000871));
#10257=CARTESIAN_POINT('Ctrl Pts',(0.159982027216266,-0.0401510462235837,
0.555571920770604));
#10258=CARTESIAN_POINT('Ctrl Pts',(-0.144657756582305,-0.0280423528175961,
0.579648625746246));
#10259=CARTESIAN_POINT('Ctrl Pts',(-0.492877605581078,-0.0114279703349173,
0.365435433134162));
#10260=CARTESIAN_POINT('Ctrl Pts',(-0.627676086705552,0.00672662241611611,
-0.0819941369368146));
#10261=CARTESIAN_POINT('Ctrl Pts',(-0.429575578790989,0.0217374029865393,
-0.411892296658343));
#10262=CARTESIAN_POINT('Ctrl Pts',(-0.152541695249049,0.0350886859058673,
-0.56523975267364));
#10263=CARTESIAN_POINT('Ctrl Pts',(0.135336383264751,0.0468071272484516,
-0.593307263800836));
#10264=CARTESIAN_POINT('Ctrl Pts',(0.458283899799568,0.0619230940080691,
-0.402587697314557));
#10265=CARTESIAN_POINT('Ctrl Pts',(0.609307758332133,0.077097462503894,
-0.0592237153848371));
#10266=CARTESIAN_POINT('Ctrl Pts',(0.53091310472218,0.0923272352205907,
0.30951522266531));
#10267=CARTESIAN_POINT('Ctrl Pts',(0.250724840721133,0.107614236320416,
0.56358297032994));
#10268=CARTESIAN_POINT('Ctrl Pts',(-0.126564120826802,0.122958232514227,
0.606014156402225));
#10269=CARTESIAN_POINT('Ctrl Pts',(-0.458600282429894,0.138360004467555,
0.419510886459279));
#10270=CARTESIAN_POINT('Ctrl Pts',(-0.61983176300993,0.153819591463941,
0.0719351225364332));
#10271=CARTESIAN_POINT('Ctrl Pts',(-0.554725504055214,0.167613443003585,
-0.26206181260559));
#10272=CARTESIAN_POINT('Ctrl Pts',(-0.310462228378986,0.18317983125893,
-0.547935611146063));
#10273=CARTESIAN_POINT('Ctrl Pts',(0.0780396026352433,0.198804639175307,
-0.641883892892221));
#10274=CARTESIAN_POINT('Ctrl Pts',(0.402026461102164,0.213627244123688,
-0.466519201503654));
#10275=CARTESIAN_POINT('Ctrl Pts',(0.544500361878148,0.224119082495714,
-0.261427818401927));
#10276=CARTESIAN_POINT('Ctrl Pts',(0.631628180764258,0.236382465082763,
0.0179423588092262));
#10277=CARTESIAN_POINT('Ctrl Pts',(0.516068994702346,0.253084696239743,
0.43193949622819));
#10278=CARTESIAN_POINT('Ctrl Pts',(0.0830210067449421,0.271930051773854,
0.646718419920737));
#10279=CARTESIAN_POINT('Ctrl Pts',(-0.312319178997566,0.288487979610228,
0.553307648248391));
#10280=CARTESIAN_POINT('Ctrl Pts',(-0.558279343154951,0.302727304137082,
0.307199029471688));
#10281=CARTESIAN_POINT('Ctrl Pts',(-0.653150400467482,0.319394308864648,
-0.0905802609109041));
#10282=CARTESIAN_POINT('Ctrl Pts',(-0.435122300634288,0.338520769864014,
-0.530070043401227));
#10283=CARTESIAN_POINT('Ctrl Pts',(0.100253391623782,0.360142020853588,
-0.681852822886023));
#10284=CARTESIAN_POINT('Ctrl Pts',(0.574125670286231,0.381867358768597,
-0.386613915232585));
#10285=CARTESIAN_POINT('Ctrl Pts',(0.675859963797566,0.403696019921949,
0.164969837630149));
#10286=CARTESIAN_POINT('Ctrl Pts',(0.333933833613938,0.425627009534933,
0.614092428525758));
#10287=CARTESIAN_POINT('Ctrl Pts',(-0.166855205845708,0.445212279958248,
0.65692348919662));
#10288=CARTESIAN_POINT('Ctrl Pts',(-0.512558158344907,0.462413615711228,
0.415370766303966));
#10289=CARTESIAN_POINT('Ctrl Pts',(-0.656905926926602,0.477202142388953,
0.0837178575488728));
#10290=CARTESIAN_POINT('Ctrl Pts',(-0.603934505805005,0.492035035282177,
-0.275965254620774));
#10291=CARTESIAN_POINT('Ctrl Pts',(-0.369111319436882,0.506911682404455,
-0.554385455958002));
#10292=CARTESIAN_POINT('Ctrl Pts',(-0.0215858718780792,0.521830986548816,
-0.667388550146379));
#10293=CARTESIAN_POINT('Ctrl Pts',(0.304496254884779,0.535546504631584,
-0.587631913783192));
#10294=CARTESIAN_POINT('Ctrl Pts',(0.529545529977474,0.548045825828215,
-0.387548801059109));
#10295=CARTESIAN_POINT('Ctrl Pts',(0.623430443923589,0.557440707689041,
-0.181835303568542));
#10296=CARTESIAN_POINT('Ctrl Pts',(0.654525025820574,0.568730207876573,
0.0836616613355354));
#10297=CARTESIAN_POINT('Ctrl Pts',(0.546500532924433,0.583818709910893,
0.44112976816762));
#10298=CARTESIAN_POINT('Ctrl Pts',(0.0884276227330822,0.604628824848464,
0.717869648196326));
#10299=CARTESIAN_POINT('Ctrl Pts',(-0.303138377589476,0.620555783445757,
0.601189590057862));
#10300=CARTESIAN_POINT('Ctrl Pts',(-0.459533951528957,0.629587879697291,
0.456235628332994));
#10301=CARTESIAN_POINT('Ctrl Pts',(-0.50533803825867,0.632441864943015,
0.406825610307984));
#10302=CARTESIAN_POINT('Ctrl Pts',(-0.574730547818871,0.637413806305203,
0.311344471281228));
#10303=CARTESIAN_POINT('Ctrl Pts',(-0.668366929241738,0.647578784537745,
0.0911858923259072));
#10304=CARTESIAN_POINT('Ctrl Pts',(-0.646014473739158,0.65869166785039,
-0.191884936486334));
#10305=CARTESIAN_POINT('Ctrl Pts',(-0.507750145831133,0.670756048992164,
-0.426018471870812));
#10306=CARTESIAN_POINT('Ctrl Pts',(-0.373964063037016,0.677176230628601,
-0.540642005287599));
#10307=CARTESIAN_POINT('Ctrl Pts',(-0.254981157617524,0.683225428963242,
-0.603522442720417));
#10308=CARTESIAN_POINT('Ctrl Pts',(-0.131378135817476,0.690256652979596,
-0.644880665656916));
#10309=CARTESIAN_POINT('Ctrl Pts',(0.0329691754781826,0.696925078957068,
-0.658603602643401));
#10310=CARTESIAN_POINT('Ctrl Pts',(0.286311574187696,0.695426723316108,
-0.654719844645462));
#10311=CARTESIAN_POINT('Ctrl Pts',(0.544469594489569,0.693381861459456,
-0.651898559429127));
#10312=CARTESIAN_POINT('Ctrl Pts',(0.779152740415451,0.69469615002134,-0.653791516275892));
#10313=CARTESIAN_POINT('Ctrl Pts',(1.1039892584626,0.694787852059779,-0.653948652768477));
#10314=CARTESIAN_POINT('Ctrl Pts',(1.51465812889679,0.694162579938424,-0.653012801319326));
#10315=CARTESIAN_POINT('Ctrl Pts',(1.83619183360445,0.694715125341329,-0.653830098307572));
#10316=CARTESIAN_POINT('Ctrl Pts',(2.00001383877787,0.69454111576742,-0.653575174848417));
#10317=CARTESIAN_POINT('Ctrl Pts',(0.584637750521914,-0.08002395673696,
-2.00006109519124));
#10318=CARTESIAN_POINT('Ctrl Pts',(0.584892738797937,-0.0801980105577937,
-1.8361974307128));
#10319=CARTESIAN_POINT('Ctrl Pts',(0.584070397282088,-0.0796469480362867,
-1.51453692100759));
#10320=CARTESIAN_POINT('Ctrl Pts',(0.585018211080981,-0.0802707046782126,
-1.1041699139982));
#10321=CARTESIAN_POINT('Ctrl Pts',(0.584844996796074,-0.0801826160882838,
-0.778992437761296));
#10322=CARTESIAN_POINT('Ctrl Pts',(0.582985364027564,-0.0788618850869893,
-0.544357823369232));
#10323=CARTESIAN_POINT('Ctrl Pts',(0.585729490711569,-0.0809239026814745,
-0.287182445226095));
#10324=CARTESIAN_POINT('Ctrl Pts',(0.589793240758398,-0.0823871514823907,
-0.0312569796179479));
#10325=CARTESIAN_POINT('Ctrl Pts',(0.575734031344313,-0.0758293347541534,
0.127340192047422));
#10326=CARTESIAN_POINT('Ctrl Pts',(0.53929719150208,-0.0696886811244117,
0.235037197670799));
#10327=CARTESIAN_POINT('Ctrl Pts',(0.483661895232482,-0.0643117779926539,
0.34091138833042));
#10328=CARTESIAN_POINT('Ctrl Pts',(0.379664997426553,-0.0584729700266611,
0.462212370815084));
#10329=CARTESIAN_POINT('Ctrl Pts',(0.168542708401427,-0.047636339134619,
0.587046009527204));
#10330=CARTESIAN_POINT('Ctrl Pts',(-0.152794966025498,-0.0348665665151376,
0.612175506111687));
#10331=CARTESIAN_POINT('Ctrl Pts',(-0.520842009334159,-0.0173073404504013,
0.386082361511922));
#10332=CARTESIAN_POINT('Ctrl Pts',(-0.663102892972978,0.00186395157458001,
-0.0866757237069638));
#10333=CARTESIAN_POINT('Ctrl Pts',(-0.453880008015841,0.0177235441027429,
-0.43515135255674));
#10334=CARTESIAN_POINT('Ctrl Pts',(-0.16119947896275,0.0318277200001107,
-0.597156692749208));
#10335=CARTESIAN_POINT('Ctrl Pts',(0.142901948310622,0.0442065744211116,
-0.626805484406487));
#10336=CARTESIAN_POINT('Ctrl Pts',(0.484028873946432,0.0601725007801429,
-0.425346166029852));
#10337=CARTESIAN_POINT('Ctrl Pts',(0.64352739507206,0.076198816494571,-0.0626916547305078));
#10338=CARTESIAN_POINT('Ctrl Pts',(0.560732644738571,0.0922807699482088,
0.326694597075312));
#10339=CARTESIAN_POINT('Ctrl Pts',(0.264900550785045,0.10842022799673,0.594929934911429));
#10340=CARTESIAN_POINT('Ctrl Pts',(-0.133349595055407,0.124616065358542,
0.639702884880681));
#10341=CARTESIAN_POINT('Ctrl Pts',(-0.483729766009194,0.140868429202419,
0.44287706510078));
#10342=CARTESIAN_POINT('Ctrl Pts',(-0.653802167228336,0.157176940491362,
0.0761921198620269));
#10343=CARTESIAN_POINT('Ctrl Pts',(-0.585125253714795,0.1717230801425,-0.276029079282174));
#10344=CARTESIAN_POINT('Ctrl Pts',(-0.327594459642905,0.188133786310116,
-0.577413377015519));
#10345=CARTESIAN_POINT('Ctrl Pts',(0.0818436386059794,0.204599843588814,
-0.676376077840266));
#10346=CARTESIAN_POINT('Ctrl Pts',(0.42307468801898,0.220211419499024,-0.491639799509712));
#10347=CARTESIAN_POINT('Ctrl Pts',(0.573088642458679,0.231258603176657,
-0.275687846185668));
#10348=CARTESIAN_POINT('Ctrl Pts',(0.664802204520714,0.244168010899022,
0.0184100054477792));
#10349=CARTESIAN_POINT('Ctrl Pts',(0.543155274881692,0.261739774606017,
0.453979428564444));
#10350=CARTESIAN_POINT('Ctrl Pts',(0.0878072781540096,0.281553832833368,
0.679729956787184));
#10351=CARTESIAN_POINT('Ctrl Pts',(-0.327583247797146,0.298951444403642,
0.581549148575783));
#10352=CARTESIAN_POINT('Ctrl Pts',(-0.585861055188208,0.313904711917007,
0.32307448664383));
#10353=CARTESIAN_POINT('Ctrl Pts',(-0.685400477254159,0.331397420979625,
-0.0944339892530362));
#10354=CARTESIAN_POINT('Ctrl Pts',(-0.456648649194199,0.351455627659057,
-0.555317863446294));
#10355=CARTESIAN_POINT('Ctrl Pts',(0.104355064344254,0.374109670982164,
-0.714240744447354));
#10356=CARTESIAN_POINT('Ctrl Pts',(0.600325552444107,0.396850329478333,
-0.40508685912858));
#10357=CARTESIAN_POINT('Ctrl Pts',(0.706584395423094,0.419675484364605,
0.171729518407216));
#10358=CARTESIAN_POINT('Ctrl Pts',(0.34930514669001,0.44258333888256,0.640786410100714));
#10359=CARTESIAN_POINT('Ctrl Pts',(-0.17322023746871,0.463017272571361,
0.685360699154325));
#10360=CARTESIAN_POINT('Ctrl Pts',(-0.533554981839275,0.480948121262819,
0.433520010328514));
#10361=CARTESIAN_POINT('Ctrl Pts',(-0.683875307228172,0.496351419981493,
0.0880553591433872));
#10362=CARTESIAN_POINT('Ctrl Pts',(-0.628700661609138,0.511787915912003,
-0.28627172728474));
#10363=CARTESIAN_POINT('Ctrl Pts',(-0.384483316527052,0.527257112128013,
-0.575768939686068));
#10364=CARTESIAN_POINT('Ctrl Pts',(-0.0233796950368831,0.542758397070066,
-0.693135592308099));
#10365=CARTESIAN_POINT('Ctrl Pts',(0.315129613443997,0.556996626383038,
-0.610300901439449));
#10366=CARTESIAN_POINT('Ctrl Pts',(0.548563681096053,0.569962296360195,
-0.402727787084418));
#10367=CARTESIAN_POINT('Ctrl Pts',(0.645875656884303,0.579701111353387,
-0.189469234165643));
#10368=CARTESIAN_POINT('Ctrl Pts',(0.678087402227607,0.591399053727189,
0.0856332935540037));
#10369=CARTESIAN_POINT('Ctrl Pts',(0.566180342756128,0.607021306882514,
0.455764435882692));
#10370=CARTESIAN_POINT('Ctrl Pts',(0.0923367089252467,0.628543104862909,
0.741820632313748));
#10371=CARTESIAN_POINT('Ctrl Pts',(-0.311985282045994,0.644989463074714,
0.621215254019459));
#10372=CARTESIAN_POINT('Ctrl Pts',(-0.473404249561221,0.654311438758149,
0.47160992481743));
#10373=CARTESIAN_POINT('Ctrl Pts',(-0.520670030114206,0.65725685157747,
0.420614920065451));
#10374=CARTESIAN_POINT('Ctrl Pts',(-0.592248587258343,0.662383411221966,
0.322168780482819));
#10375=CARTESIAN_POINT('Ctrl Pts',(-0.688734911720638,0.672871119021292,
0.0950038824064079));
#10376=CARTESIAN_POINT('Ctrl Pts',(-0.665867604510835,0.684306259795084,
-0.196319960324102));
#10377=CARTESIAN_POINT('Ctrl Pts',(-0.523264547581101,0.696742034629231,
-0.43769269867827));
#10378=CARTESIAN_POINT('Ctrl Pts',(-0.385571678876014,0.703352498122265,
-0.555622128823214));
#10379=CARTESIAN_POINT('Ctrl Pts',(-0.263639834025884,0.709548173405927,
-0.620061658738199));
#10380=CARTESIAN_POINT('Ctrl Pts',(-0.13596345065982,0.716817624310851,
-0.662808505090214));
#10381=CARTESIAN_POINT('Ctrl Pts',(0.0328701126263124,0.723623474439416,
-0.67673682834849));
#10382=CARTESIAN_POINT('Ctrl Pts',(0.286974825485283,0.722084330497799,
-0.672795432729989));
#10383=CARTESIAN_POINT('Ctrl Pts',(0.544470548836667,0.720058117306266,
-0.669996370718004));
#10384=CARTESIAN_POINT('Ctrl Pts',(0.778866262009698,0.721364810413718,
-0.671878222247616));
#10385=CARTESIAN_POINT('Ctrl Pts',(1.10424366248717,0.721460534244764,-0.672039567606643));
#10386=CARTESIAN_POINT('Ctrl Pts',(1.51446664209188,0.72083249825408,-0.671098379809243));
#10387=CARTESIAN_POINT('Ctrl Pts',(1.83619853648755,0.721386379956638,-0.671916335232525));
#10388=CARTESIAN_POINT('Ctrl Pts',(2.00007031245355,0.72121231751685,-0.671661334325028));
#10389=CARTESIAN_POINT('Ctrl Pts',(0.600124355483138,-0.0799998580128369,
-2.00008516830249));
#10390=CARTESIAN_POINT('Ctrl Pts',(0.600379376695529,-0.0801739343158842,
-1.83620033785433));
#10391=CARTESIAN_POINT('Ctrl Pts',(0.599557188536607,-0.0796220546015198,
-1.51445131895255));
#10392=CARTESIAN_POINT('Ctrl Pts',(0.60050657815397,-0.0802473516234908,
-1.10427966986787));
#10393=CARTESIAN_POINT('Ctrl Pts',(0.600332768539301,-0.0801568850586992,
-0.778861249100346));
#10394=CARTESIAN_POINT('Ctrl Pts',(0.598475600091931,-0.078840606257744,
-0.544366061842844));
#10395=CARTESIAN_POINT('Ctrl Pts',(0.601215825651616,-0.0808915608655967,
-0.287431516632137));
#10396=CARTESIAN_POINT('Ctrl Pts',(0.605291661148957,-0.0823787912019986,
-0.0313608552946517));
#10397=CARTESIAN_POINT('Ctrl Pts',(0.59116069745846,-0.0757414785640243,
0.130026789470337));
#10398=CARTESIAN_POINT('Ctrl Pts',(0.553569673303418,-0.0693986540389958,
0.241244525168603));
#10399=CARTESIAN_POINT('Ctrl Pts',(0.49648068595625,-0.0638861429178919,
0.349817593838996));
#10400=CARTESIAN_POINT('Ctrl Pts',(0.389834766749766,-0.0578962864213881,
0.474234392676377));
#10401=CARTESIAN_POINT('Ctrl Pts',(0.172953767301598,-0.0467647821330201,
0.602517389648945));
#10402=CARTESIAN_POINT('Ctrl Pts',(-0.156611161701388,-0.033669257315275,
0.62816084010969));
#10403=CARTESIAN_POINT('Ctrl Pts',(-0.534324881784356,-0.0156487609275952,
0.396251684871875));
#10404=CARTESIAN_POINT('Ctrl Pts',(-0.680173923436771,0.00401467962268951,
-0.0887673006211078));
#10405=CARTESIAN_POINT('Ctrl Pts',(-0.465603920420951,0.020280840108104,
-0.446125545894049));
#10406=CARTESIAN_POINT('Ctrl Pts',(-0.16548447812985,0.0347430378954353,
-0.612246576434715));
#10407=CARTESIAN_POINT('Ctrl Pts',(0.146296739212227,0.0474345780356556,
-0.642633153997123));
#10408=CARTESIAN_POINT('Ctrl Pts',(0.495951952987202,0.063799790307997,
-0.436120013454043));
#10409=CARTESIAN_POINT('Ctrl Pts',(0.659386574747031,0.0802231528742134,
-0.0644747476625062));
#10410=CARTESIAN_POINT('Ctrl Pts',(0.574545975795925,0.0966991624308195,
0.334451049923668));
#10411=CARTESIAN_POINT('Ctrl Pts',(0.271532980288635,0.11322968614674,0.60917227723542));
#10412=CARTESIAN_POINT('Ctrl Pts',(-0.136251703472976,0.12981319447486,
0.654997709328214));
#10413=CARTESIAN_POINT('Ctrl Pts',(-0.494901469661726,0.146449568036652,
0.45350333530914));
#10414=CARTESIAN_POINT('Ctrl Pts',(-0.668917235906318,0.163138202692549,
0.0782626975824873));
#10415=CARTESIAN_POINT('Ctrl Pts',(-0.598645464166764,0.178018515644393,
-0.282045078558144));
#10416=CARTESIAN_POINT('Ctrl Pts',(-0.335262469427464,0.194801446585974,
-0.590258155385672));
#10417=CARTESIAN_POINT('Ctrl Pts',(0.0833245701146875,0.211635076942448,
-0.691392401965039));
#10418=CARTESIAN_POINT('Ctrl Pts',(0.432010324368538,0.227588445577569,
-0.502588887028728));
#10419=CARTESIAN_POINT('Ctrl Pts',(0.585260109788594,0.238874210076111,
-0.281973448384831));
#10420=CARTESIAN_POINT('Ctrl Pts',(0.678932070081789,0.25205984880311,0.018422105283869));
#10421=CARTESIAN_POINT('Ctrl Pts',(0.55467369883675,0.270001497383997,0.463140844788188));
#10422=CARTESIAN_POINT('Ctrl Pts',(0.0899761556469263,0.290221466632431,
0.693463094883412));
#10423=CARTESIAN_POINT('Ctrl Pts',(-0.33371627867329,0.307967186991324,
0.593293078602062));
#10424=CARTESIAN_POINT('Ctrl Pts',(-0.59704764533906,0.323213852266529,
0.329736222807235));
#10425=CARTESIAN_POINT('Ctrl Pts',(-0.698474654722095,0.341042833941317,
-0.0958055766422671));
#10426=CARTESIAN_POINT('Ctrl Pts',(-0.465383647491834,0.361476669823075,
-0.565288791036093));
#10427=CARTESIAN_POINT('Ctrl Pts',(0.105790956320368,0.384540697804113,
-0.727009690342144));
#10428=CARTESIAN_POINT('Ctrl Pts',(0.610371558079431,0.407678360937913,
-0.412394382377907));
#10429=CARTESIAN_POINT('Ctrl Pts',(0.718333583382585,0.43088704560672,0.174123208014002));
#10430=CARTESIAN_POINT('Ctrl Pts',(0.355226639142397,0.454164351268278,
0.650688896190773));
#10431=CARTESIAN_POINT('Ctrl Pts',(-0.17537106718635,0.474914221668976,
0.695875511358292));
#10432=CARTESIAN_POINT('Ctrl Pts',(-0.54103585275066,0.493111378816631,
0.440272937100537));
#10433=CARTESIAN_POINT('Ctrl Pts',(-0.6934950282823,0.508736295299708,0.0898302457491503));
#10434=CARTESIAN_POINT('Ctrl Pts',(-0.637526970610404,0.524387740772898,
-0.289700706598419));
#10435=CARTESIAN_POINT('Ctrl Pts',(-0.390008311550144,0.540064979323309,
-0.583068679337088));
#10436=CARTESIAN_POINT('Ctrl Pts',(-0.024226148296103,0.555766910199861,
-0.701929930807063));
#10437=CARTESIAN_POINT('Ctrl Pts',(0.318491600824293,0.570182538995617,
-0.618039769051569));
#10438=CARTESIAN_POINT('Ctrl Pts',(0.554723176441453,0.583304202833105,
-0.40796362014035));
#10439=CARTESIAN_POINT('Ctrl Pts',(0.653160192073423,0.593156620195102,
-0.192217361281352));
#10440=CARTESIAN_POINT('Ctrl Pts',(0.685736178259883,0.60498732605382,0.0860074066354565));
#10441=CARTESIAN_POINT('Ctrl Pts',(0.572562677668091,0.620781559492554,
0.4602016432688));
#10442=CARTESIAN_POINT('Ctrl Pts',(0.0937765103860463,0.642526123974182,
0.7491364099364));
#10443=CARTESIAN_POINT('Ctrl Pts',(-0.314388630844237,0.659130029858254,
0.627315372568153));
#10444=CARTESIAN_POINT('Ctrl Pts',(-0.477285810697724,0.668537384089933,
0.47634220294986));
#10445=CARTESIAN_POINT('Ctrl Pts',(-0.524979531484106,0.671509580653182,
0.42488265802704));
#10446=CARTESIAN_POINT('Ctrl Pts',(-0.597194271883867,0.676681179673865,
0.325573954028726));
#10447=CARTESIAN_POINT('Ctrl Pts',(-0.694496329532521,0.687262154305694,
0.0963821879712936));
#10448=CARTESIAN_POINT('Ctrl Pts',(-0.671478629812927,0.698788430555515,
-0.197261795472992));
#10449=CARTESIAN_POINT('Ctrl Pts',(-0.527677507863671,0.71132631016803,
-0.440626908636377));
#10450=CARTESIAN_POINT('Ctrl Pts',(-0.388905141275015,0.717990004861966,
-0.559470705037612));
#10451=CARTESIAN_POINT('Ctrl Pts',(-0.266282257094333,0.724219498671225,
-0.624266154108112));
#10452=CARTESIAN_POINT('Ctrl Pts',(-0.13757925918983,0.731550254164043,
-0.667380131292113));
#10453=CARTESIAN_POINT('Ctrl Pts',(0.0327675186379925,0.738404779593333,
-0.681400099587548));
#10454=CARTESIAN_POINT('Ctrl Pts',(0.28724639971344,0.736851511264604,-0.677433025330373));
#10455=CARTESIAN_POINT('Ctrl Pts',(0.544462158077268,0.734831948662016,
-0.674646491228074));
#10456=CARTESIAN_POINT('Ctrl Pts',(0.778748964711316,0.736136065865045,
-0.676524055782765));
#10457=CARTESIAN_POINT('Ctrl Pts',(1.10434282010243,0.736233268880018,-0.676688327154564));
#10458=CARTESIAN_POINT('Ctrl Pts',(1.51438929680924,0.735604358561319,-0.675746079653723));
#10459=CARTESIAN_POINT('Ctrl Pts',(1.83620130898864,0.736158775205925,-0.676565295388705));
#10460=CARTESIAN_POINT('Ctrl Pts',(2.00009323767342,0.735984691360185,-0.676310263121558));
#10461=CARTESIAN_POINT('Origin',(0.6,0.,-2.));
#10462=CARTESIAN_POINT('Origin',(1.99999999999998,0.759999999999999,-0.60000000000007));
#10463=CARTESIAN_POINT('Origin',(1.99999999999998,0.759999999999999,-0.60000000000007));
#10464=CARTESIAN_POINT('Origin',(0.6,0.,-2.));
#10465=CARTESIAN_POINT('',(0.,0.,0.));
#10466=CARTESIAN_POINT('',(0.,0.,0.));
#10467=CARTESIAN_POINT('',(0.,0.,0.));
#10468=CARTESIAN_POINT('',(0.,0.,0.));
#10469=CARTESIAN_POINT('',(0.,0.,0.));
#10470=CARTESIAN_POINT('',(0.,0.,0.));
#10471=CARTESIAN_POINT('',(0.,0.,0.));
#10472=CARTESIAN_POINT('',(0.,0.,0.));
#10473=CARTESIAN_POINT('',(0.,0.,0.));
#10474=CARTESIAN_POINT('',(0.,0.,2.5));
#10475=CARTESIAN_POINT('',(1.76776695296637,1.76776695296637,1.8));
#10476=CARTESIAN_POINT('',(1.23743686707646,1.23743686707646,4.));
#10477=CARTESIAN_POINT('',(-1.76776695296637,1.76776695296637,1.8));
#10478=CARTESIAN_POINT('',(-1.23743686707646,1.23743686707646,4.));
#10479=CARTESIAN_POINT('',(-1.76776695296637,-1.76776695296637,1.8));
#10480=CARTESIAN_POINT('',(-1.23743686707646,-1.23743686707646,4.));
#10481=CARTESIAN_POINT('',(1.76776695296637,-1.76776695296637,1.8));
#10482=CARTESIAN_POINT('',(1.23743686707646,-1.23743686707646,4.));
#10483=CARTESIAN_POINT('',(5.1,-3.47,1.8));
#10484=CARTESIAN_POINT('',(7.9,-3.47,1.8));
#10485=CARTESIAN_POINT('',(6.5,-3.47,6.84));
#10486=CARTESIAN_POINT('',(8.8,-2.47,0.));
#10487=CARTESIAN_POINT('',(6.5,-3.47,5.6));
#10488=CARTESIAN_POINT('',(0.,0.,0.));
#10489=CARTESIAN_POINT('',(0.,0.,0.));
#10490=CARTESIAN_POINT('Origin',(0.,0.,4.8));
#10491=CARTESIAN_POINT('',(-1.,-1.22464679914735E-16,4.8));
#10492=CARTESIAN_POINT('Origin',(0.,0.,4.8));
#10493=CARTESIAN_POINT('',(-0.7,-8.57252759403147E-17,4.8));
#10494=CARTESIAN_POINT('Origin',(0.,0.,4.8));
#10495=CARTESIAN_POINT('Origin',(0.,0.,4.8));
#10496=CARTESIAN_POINT('',(-1.,-1.22464679914735E-16,6.4));
#10497=CARTESIAN_POINT('Origin',(0.,0.,6.4));
#10498=CARTESIAN_POINT('',(-1.,-1.22464679914735E-16,4.8));
#10499=CARTESIAN_POINT('Origin',(0.,0.,2.95));
#10500=CARTESIAN_POINT('',(-0.7,-8.57252759403147E-17,2.95));
#10501=CARTESIAN_POINT('Origin',(0.,0.,2.95));
#10502=CARTESIAN_POINT('',(-0.5,6.12323399573677E-17,2.95));
#10503=CARTESIAN_POINT('Origin',(0.,0.,2.95));
#10504=CARTESIAN_POINT('Origin',(0.,0.,2.95));
#10505=CARTESIAN_POINT('',(-0.7,-8.57252759403147E-17,2.95));
#10506=CARTESIAN_POINT('Origin',(0.,0.,1.));
#10507=CARTESIAN_POINT('',(-0.5,-6.12323399573677E-17,1.));
#10508=CARTESIAN_POINT('',(-0.5,-6.12323399573677E-17,1.));
#10509=CARTESIAN_POINT('Origin',(0.,0.,1.));
#10510=CARTESIAN_POINT('Origin',(0.,0.,6.4));
#10511=CARTESIAN_POINT('Origin',(0.,0.,1.));
#10512=CARTESIAN_POINT('',(0.,0.,0.));
#10513=CARTESIAN_POINT('Origin',(0.,0.,1.8));
#10514=CARTESIAN_POINT('',(-0.505,-6.18446633569413E-17,2.05));
#10515=CARTESIAN_POINT('Origin',(0.,0.,2.05));
#10516=CARTESIAN_POINT('',(-0.505,-6.18446633569413E-17,1.8));
#10517=CARTESIAN_POINT('',(-0.505,-6.18446633569413E-17,1.8));
#10518=CARTESIAN_POINT('Origin',(0.,0.,1.8));
#10519=CARTESIAN_POINT('Origin',(0.,0.,1.8));
#10520=CARTESIAN_POINT('',(-0.7,-8.57252759403147E-17,2.05));
#10521=CARTESIAN_POINT('Origin',(0.,0.,2.05));
#10522=CARTESIAN_POINT('',(-0.7,-8.57252759403147E-17,1.8));
#10523=CARTESIAN_POINT('',(-0.7,-8.57252759403147E-17,1.8));
#10524=CARTESIAN_POINT('Origin',(0.,0.,1.8));
#10525=CARTESIAN_POINT('Origin',(0.,0.,2.05));
#10526=CARTESIAN_POINT('Origin',(0.,0.,1.8));
#10527=CARTESIAN_POINT('',(0.,0.,0.));
#10528=CARTESIAN_POINT('Origin',(0.49,0.,1.4));
#10529=CARTESIAN_POINT('',(0.49,0.122167917228706,1.28909463493591));
#10530=CARTESIAN_POINT('',(0.49,0.122167917228706,1.51090536506409));
#10531=CARTESIAN_POINT('',(0.49,0.122167917228706,1.));
#10532=CARTESIAN_POINT('Origin',(0.49,0.,1.4));
#10533=CARTESIAN_POINT('Origin',(0.49,0.,1.4));
#10534=CARTESIAN_POINT('',(0.49,-0.122167917228706,1.28909463493591));
#10535=CARTESIAN_POINT('Ctrl Pts',(0.49,-0.122167917228706,1.28909463493591));
#10536=CARTESIAN_POINT('Ctrl Pts',(0.490448531679987,-0.120368913626296,
1.28711294069536));
#10537=CARTESIAN_POINT('Ctrl Pts',(0.490895245371685,-0.118534896565231,
1.28518965877367));
#10538=CARTESIAN_POINT('Ctrl Pts',(0.494795015531646,-0.102111993019358,
1.2687667552278));
#10539=CARTESIAN_POINT('Ctrl Pts',(0.498442514607594,-0.0836597150224318,
1.25609154388858));
#10540=CARTESIAN_POINT('Ctrl Pts',(0.50357781976106,-0.0430495960471595,
1.23920409039234));
#10541=CARTESIAN_POINT('Ctrl Pts',(0.505,-0.020880094330741,1.235));
#10542=CARTESIAN_POINT('Ctrl Pts',(0.505,0.020880094330741,1.235));
#10543=CARTESIAN_POINT('Ctrl Pts',(0.50357781976106,0.0430495960471595,
1.23920409039234));
#10544=CARTESIAN_POINT('Ctrl Pts',(0.498442514607594,0.0836597150224318,
1.25609154388858));
#10545=CARTESIAN_POINT('Ctrl Pts',(0.494795015531646,0.102111993019358,
1.2687667552278));
#10546=CARTESIAN_POINT('Ctrl Pts',(0.490895245371684,0.118534896565231,
1.28518965877367));
#10547=CARTESIAN_POINT('Ctrl Pts',(0.490448531679987,0.120368913626296,
1.28711294069536));
#10548=CARTESIAN_POINT('Ctrl Pts',(0.49,0.122167917228706,1.28909463493591));
#10549=CARTESIAN_POINT('',(0.49,-0.122167917228706,1.51090536506409));
#10550=CARTESIAN_POINT('Origin',(0.49,0.,1.4));
#10551=CARTESIAN_POINT('',(0.505,-1.70422299968729E-17,1.565));
#10552=CARTESIAN_POINT('Ctrl Pts',(0.505,-6.93889390390723E-18,1.565));
#10553=CARTESIAN_POINT('Ctrl Pts',(0.505,-0.020880094330741,1.565));
#10554=CARTESIAN_POINT('Ctrl Pts',(0.50357781976106,-0.0430495960471595,
1.56079590960766));
#10555=CARTESIAN_POINT('Ctrl Pts',(0.498442514607594,-0.0836597150224318,
1.54390845611142));
#10556=CARTESIAN_POINT('Ctrl Pts',(0.494795015531646,-0.102111993019358,
1.5312332447722));
#10557=CARTESIAN_POINT('Ctrl Pts',(0.490895245371684,-0.118534896565231,
1.51481034122633));
#10558=CARTESIAN_POINT('Ctrl Pts',(0.490448531679987,-0.120368913626296,
1.51288705930464));
#10559=CARTESIAN_POINT('Ctrl Pts',(0.49,-0.122167917228706,1.51090536506409));
#10560=CARTESIAN_POINT('',(0.9,-2.02066721859313E-17,1.565));
#10561=CARTESIAN_POINT('',(0.49,-2.02066721859313E-17,1.565));
#10562=CARTESIAN_POINT('',(0.884745726183518,0.165,1.4));
#10563=CARTESIAN_POINT('Ctrl Pts',(0.884745726183518,0.165,1.4));
#10564=CARTESIAN_POINT('Ctrl Pts',(0.884745726183518,0.165,1.37923124059256));
#10565=CARTESIAN_POINT('Ctrl Pts',(0.885552759505264,0.160839719007584,
1.35711110492666));
#10566=CARTESIAN_POINT('Ctrl Pts',(0.888448648150043,0.143986470216691,
1.31647293736623));
#10567=CARTESIAN_POINT('Ctrl Pts',(0.890493604851638,0.131295993814186,
1.29795075602263));
#10568=CARTESIAN_POINT('Ctrl Pts',(0.89431723432394,0.102049819008125,1.26870458121656));
#10569=CARTESIAN_POINT('Ctrl Pts',(0.896347088899543,0.0835273920906824,
1.25601365401642));
#10570=CARTESIAN_POINT('Ctrl Pts',(0.899208271860583,0.0428883760934127,
1.23916007816136));
#10571=CARTESIAN_POINT('Ctrl Pts',(0.9,0.0207679427235068,1.235));
#10572=CARTESIAN_POINT('Ctrl Pts',(0.9,-0.0207679427235068,1.235));
#10573=CARTESIAN_POINT('Ctrl Pts',(0.899208271860583,-0.0428883760934127,
1.23916007816136));
#10574=CARTESIAN_POINT('Ctrl Pts',(0.896347088899543,-0.0835273920906823,
1.25601365401642));
#10575=CARTESIAN_POINT('Ctrl Pts',(0.89431723432394,-0.102049819008125,
1.26870458121656));
#10576=CARTESIAN_POINT('Ctrl Pts',(0.890493604851638,-0.131295993814186,
1.29795075602263));
#10577=CARTESIAN_POINT('Ctrl Pts',(0.888448648150043,-0.143986470216691,
1.31647293736623));
#10578=CARTESIAN_POINT('Ctrl Pts',(0.885552759505264,-0.160839719007584,
1.35711110492666));
#10579=CARTESIAN_POINT('Ctrl Pts',(0.884745726183518,-0.165,1.37923124059256));
#10580=CARTESIAN_POINT('Ctrl Pts',(0.884745726183518,-0.165,1.42076875940744));
#10581=CARTESIAN_POINT('Ctrl Pts',(0.885552759505264,-0.160839719007584,
1.44288889507334));
#10582=CARTESIAN_POINT('Ctrl Pts',(0.888448648150043,-0.14398647021669,
1.48352706263377));
#10583=CARTESIAN_POINT('Ctrl Pts',(0.890493604851638,-0.131295993814186,
1.50204924397737));
#10584=CARTESIAN_POINT('Ctrl Pts',(0.89431723432394,-0.102049819008125,
1.53129541878344));
#10585=CARTESIAN_POINT('Ctrl Pts',(0.896347088899543,-0.0835273920906824,
1.54398634598358));
#10586=CARTESIAN_POINT('Ctrl Pts',(0.899208271860583,-0.0428883760934128,
1.56083992183864));
#10587=CARTESIAN_POINT('Ctrl Pts',(0.9,-0.0207679427235068,1.565));
#10588=CARTESIAN_POINT('Ctrl Pts',(0.9,-6.93889390390723E-18,1.565));
#10589=CARTESIAN_POINT('Ctrl Pts',(0.9,-3.46944695195361E-17,1.565));
#10590=CARTESIAN_POINT('Ctrl Pts',(0.9,0.0207679427235068,1.565));
#10591=CARTESIAN_POINT('Ctrl Pts',(0.899208271860583,0.0428883760934127,
1.56083992183864));
#10592=CARTESIAN_POINT('Ctrl Pts',(0.896347088899543,0.0835273920906824,
1.54398634598358));
#10593=CARTESIAN_POINT('Ctrl Pts',(0.89431723432394,0.102049819008125,1.53129541878344));
#10594=CARTESIAN_POINT('Ctrl Pts',(0.890493604851638,0.131295993814186,
1.50204924397737));
#10595=CARTESIAN_POINT('Ctrl Pts',(0.888448648150043,0.143986470216691,
1.48352706263377));
#10596=CARTESIAN_POINT('Ctrl Pts',(0.885552759505264,0.160839719007584,
1.44288889507334));
#10597=CARTESIAN_POINT('Ctrl Pts',(0.884745726183518,0.165,1.42076875940744));
#10598=CARTESIAN_POINT('Ctrl Pts',(0.884745726183518,0.165,1.4));
#10599=CARTESIAN_POINT('Ctrl Pts',(0.49,0.122167917228706,1.51090536506409));
#10600=CARTESIAN_POINT('Ctrl Pts',(0.490448531679987,0.120368913626296,
1.51288705930464));
#10601=CARTESIAN_POINT('Ctrl Pts',(0.490895245371685,0.118534896565231,
1.51481034122633));
#10602=CARTESIAN_POINT('Ctrl Pts',(0.494795015531646,0.102111993019358,
1.5312332447722));
#10603=CARTESIAN_POINT('Ctrl Pts',(0.498442514607594,0.0836597150224318,
1.54390845611142));
#10604=CARTESIAN_POINT('Ctrl Pts',(0.50357781976106,0.0430495960471594,
1.56079590960766));
#10605=CARTESIAN_POINT('Ctrl Pts',(0.505,0.020880094330741,1.565));
#10606=CARTESIAN_POINT('Ctrl Pts',(0.505,0.,1.565));
#10607=CARTESIAN_POINT('Origin',(0.49,0.,1.4));
#10608=CARTESIAN_POINT('',(0.49,-0.122167917228706,1.));
#10609=CARTESIAN_POINT('Origin',(0.,0.,1.));
#10610=CARTESIAN_POINT('',(-0.505,-6.18446633569413E-17,1.8));
#10611=CARTESIAN_POINT('Origin',(0.,0.,1.8));
#10612=CARTESIAN_POINT('',(-0.505,-6.18446633569413E-17,1.));
#10613=CARTESIAN_POINT('',(-0.505,-6.18446633569413E-17,1.));
#10614=CARTESIAN_POINT('Origin',(0.,0.,1.));
#10615=CARTESIAN_POINT('Origin',(0.,0.,1.));
#10616=CARTESIAN_POINT('',(-0.9,-1.10218211923262E-16,1.8));
#10617=CARTESIAN_POINT('Origin',(0.,0.,1.8));
#10618=CARTESIAN_POINT('',(-0.9,-1.10218211923262E-16,1.));
#10619=CARTESIAN_POINT('',(-0.9,-1.10218211923262E-16,1.));
#10620=CARTESIAN_POINT('Origin',(0.,0.,1.));
#10621=CARTESIAN_POINT('Origin',(0.,0.,1.8));
#10622=CARTESIAN_POINT('Origin',(0.,0.,1.));
#10623=CARTESIAN_POINT('',(0.,0.,0.));
#10624=CARTESIAN_POINT('Origin',(0.,-0.4,0.));
#10625=CARTESIAN_POINT('',(-0.1954,-0.4,2.39295984553393E-17));
#10626=CARTESIAN_POINT('Origin',(0.,-0.4,0.));
#10627=CARTESIAN_POINT('Origin',(0.0577350269189626,0.,-0.1));
#10628=CARTESIAN_POINT('',(0.0577350269189626,0.,-0.1));
#10629=CARTESIAN_POINT('',(0.115470053837925,0.,0.));
#10630=CARTESIAN_POINT('',(0.0934187836487032,0.,-0.0381939203391614));
#10631=CARTESIAN_POINT('',(0.0577350269189626,-0.2,-0.1));
#10632=CARTESIAN_POINT('',(0.0577350269189626,0.,-0.1));
#10633=CARTESIAN_POINT('',(0.115470053837925,-0.2,0.));
#10634=CARTESIAN_POINT('',(0.115470053837925,-0.2,0.));
#10635=CARTESIAN_POINT('',(0.115470053837925,0.,0.));
#10636=CARTESIAN_POINT('Origin',(-0.0577350269189626,0.,-0.1));
#10637=CARTESIAN_POINT('',(-0.0577350269189626,0.,-0.1));
#10638=CARTESIAN_POINT('',(0.0561324865405187,0.,-0.1));
#10639=CARTESIAN_POINT('',(-0.0577350269189626,-0.2,-0.1));
#10640=CARTESIAN_POINT('',(-0.0577350269189626,0.,-0.1));
#10641=CARTESIAN_POINT('',(0.0577350269189626,-0.2,-0.1));
#10642=CARTESIAN_POINT('Origin',(-0.115470053837925,0.,-1.38777878078145E-17));
#10643=CARTESIAN_POINT('',(-0.115470053837925,0.,-1.41410031829988E-17));
#10644=CARTESIAN_POINT('',(-0.0797862971081845,0.,-0.0618060796608387));
#10645=CARTESIAN_POINT('',(-0.115470053837925,-0.2,-1.38777878078145E-17));
#10646=CARTESIAN_POINT('',(-0.115470053837925,0.,-1.41410031829988E-17));
#10647=CARTESIAN_POINT('',(-0.0577350269189626,-0.2,-0.1));
#10648=CARTESIAN_POINT('Origin',(-0.0577350269189626,0.,0.1));
#10649=CARTESIAN_POINT('',(-0.0577350269189626,0.,0.1));
#10650=CARTESIAN_POINT('',(-0.0509187836487033,0.,0.111806079660839));
#10651=CARTESIAN_POINT('',(-0.0577350269189626,-0.2,0.1));
#10652=CARTESIAN_POINT('',(-0.0577350269189626,0.,0.1));
#10653=CARTESIAN_POINT('',(-0.115470053837925,-0.2,-1.41410031829988E-17));
#10654=CARTESIAN_POINT('Origin',(0.0577350269189626,0.,0.1));
#10655=CARTESIAN_POINT('',(0.0577350269189626,0.,0.1));
#10656=CARTESIAN_POINT('',(0.113867513459481,0.,0.1));
#10657=CARTESIAN_POINT('',(0.0577350269189626,-0.2,0.1));
#10658=CARTESIAN_POINT('',(0.0577350269189626,0.,0.1));
#10659=CARTESIAN_POINT('',(-0.0577350269189626,-0.2,0.1));
#10660=CARTESIAN_POINT('Origin',(0.115470053837925,0.,0.));
#10661=CARTESIAN_POINT('',(0.122286297108185,0.,-0.0118060796608386));
#10662=CARTESIAN_POINT('',(0.0577350269189626,-0.2,0.1));
#10663=CARTESIAN_POINT('Origin',(0.,-0.2,0.));
#10664=CARTESIAN_POINT('Origin',(0.17,0.,0.));
#10665=CARTESIAN_POINT('',(-0.17,-8.67361737988404E-18,-2.0818995585505E-17));
#10666=CARTESIAN_POINT('Origin',(0.,0.,0.));
#10667=CARTESIAN_POINT('Origin',(0.,-0.015,0.));
#10668=CARTESIAN_POINT('',(-0.1954,-0.0254,-2.39295984553393E-17));
#10669=CARTESIAN_POINT('Origin',(0.,-0.0254,0.));
#10670=CARTESIAN_POINT('',(-0.185,-0.015,-2.2655965784226E-17));
#10671=CARTESIAN_POINT('Origin',(0.,-0.2775,0.));
#10672=CARTESIAN_POINT('',(-0.1954,-0.2775,-2.39295984553393E-17));
#10673=CARTESIAN_POINT('',(0.,0.,0.));
#10674=CARTESIAN_POINT('Origin',(0.,-2.4,7.52));
#10675=CARTESIAN_POINT('',(0.172988438920056,-2.51905880899792,7.52));
#10676=CARTESIAN_POINT('',(0.172988438920056,-2.28094119100208,7.52));
#10677=CARTESIAN_POINT('',(0.172988438920056,-3.6,7.52));
#10678=CARTESIAN_POINT('Origin',(0.,-2.4,7.52));
#10679=CARTESIAN_POINT('Origin',(0.,-2.4,7.52));
#10680=CARTESIAN_POINT('',(-0.172988438920056,-2.51905880899792,7.52));
#10681=CARTESIAN_POINT('Ctrl Pts',(-0.172988438920056,-2.51905880899792,
7.52));
#10682=CARTESIAN_POINT('Ctrl Pts',(-0.165594865311314,-2.52980142239529,
7.52129192197638));
#10683=CARTESIAN_POINT('Ctrl Pts',(-0.157297138725606,-2.53968770937274,
7.52265394943905));
#10684=CARTESIAN_POINT('Ctrl Pts',(-0.129892073845076,-2.56709277425327,
7.5267480843909));
#10685=CARTESIAN_POINT('Ctrl Pts',(-0.106330167759285,-2.58324205633295,
7.52969589327638));
#10686=CARTESIAN_POINT('Ctrl Pts',(-0.0546129046324105,-2.60469779396491,
7.53385029472357));
#10687=CARTESIAN_POINT('Ctrl Pts',(-0.0264512308298517,-2.61,7.535));
#10688=CARTESIAN_POINT('Ctrl Pts',(0.0264512308298516,-2.61,7.535));
#10689=CARTESIAN_POINT('Ctrl Pts',(0.0546129046324104,-2.60469779396491,
7.53385029472357));
#10690=CARTESIAN_POINT('Ctrl Pts',(0.106330167759284,-2.58324205633295,
7.52969589327638));
#10691=CARTESIAN_POINT('Ctrl Pts',(0.129892073845076,-2.56709277425327,
7.5267480843909));
#10692=CARTESIAN_POINT('Ctrl Pts',(0.157297138725606,-2.53968770937274,
7.52265394943905));
#10693=CARTESIAN_POINT('Ctrl Pts',(0.165594865311314,-2.52980142239529,
7.52129192197638));
#10694=CARTESIAN_POINT('Ctrl Pts',(0.172988438920056,-2.51905880899792,
7.52));
#10695=CARTESIAN_POINT('',(-0.21,-2.4,7.52));
#10696=CARTESIAN_POINT('Origin',(0.,-2.4,7.52));
#10697=CARTESIAN_POINT('',(-0.21,-2.4,8.11615888233178));
#10698=CARTESIAN_POINT('',(-0.21,-2.4,7.52));
#10699=CARTESIAN_POINT('',(0.21,-2.4,8.11615888233178));
#10700=CARTESIAN_POINT('Ctrl Pts',(0.21,-2.4,8.11615888233178));
#10701=CARTESIAN_POINT('Ctrl Pts',(0.21,-2.42640093420375,8.11615888233178));
#10702=CARTESIAN_POINT('Ctrl Pts',(0.20471752266132,-2.45454055536511,8.11688606295397));
#10703=CARTESIAN_POINT('Ctrl Pts',(0.183276841782292,-2.5062710523005,8.11950502964782));
#10704=CARTESIAN_POINT('Ctrl Pts',(0.167120287247804,-2.52986456085055,
8.12135816887013));
#10705=CARTESIAN_POINT('Ctrl Pts',(0.129864750292352,-2.567120097806,8.12483075953278));
#10706=CARTESIAN_POINT('Ctrl Pts',(0.106271159541076,-2.58327680083123,
8.12667690933009));
#10707=CARTESIAN_POINT('Ctrl Pts',(0.0545403836274688,-2.6047175903444,
8.12927985626981));
#10708=CARTESIAN_POINT('Ctrl Pts',(0.0264006657112965,-2.61,8.13));
#10709=CARTESIAN_POINT('Ctrl Pts',(-0.0264006657112964,-2.61,8.13));
#10710=CARTESIAN_POINT('Ctrl Pts',(-0.0545403836274688,-2.6047175903444,
8.12927985626981));
#10711=CARTESIAN_POINT('Ctrl Pts',(-0.106271159541076,-2.58327680083123,
8.12667690933009));
#10712=CARTESIAN_POINT('Ctrl Pts',(-0.129864750292352,-2.567120097806,8.12483075953278));
#10713=CARTESIAN_POINT('Ctrl Pts',(-0.167120287247804,-2.52986456085055,
8.12135816887013));
#10714=CARTESIAN_POINT('Ctrl Pts',(-0.183276841782292,-2.5062710523005,
8.11950502964782));
#10715=CARTESIAN_POINT('Ctrl Pts',(-0.20471752266132,-2.45454055536511,
8.11688606295397));
#10716=CARTESIAN_POINT('Ctrl Pts',(-0.21,-2.42640093420375,8.11615888233178));
#10717=CARTESIAN_POINT('Ctrl Pts',(-0.21,-2.4,8.11615888233178));
#10718=CARTESIAN_POINT('Ctrl Pts',(-0.21,-2.4,8.11615888233178));
#10719=CARTESIAN_POINT('Ctrl Pts',(-0.21,-2.37359906579625,8.11615888233178));
#10720=CARTESIAN_POINT('Ctrl Pts',(-0.20471752266132,-2.34545944463489,
8.11688606295397));
#10721=CARTESIAN_POINT('Ctrl Pts',(-0.183276841782292,-2.2937289476995,
8.11950502964782));
#10722=CARTESIAN_POINT('Ctrl Pts',(-0.167120287247804,-2.27013543914945,
8.12135816887013));
#10723=CARTESIAN_POINT('Ctrl Pts',(-0.129864750292352,-2.232879902194,8.12483075953278));
#10724=CARTESIAN_POINT('Ctrl Pts',(-0.106271159541076,-2.21672319916877,
8.12667690933009));
#10725=CARTESIAN_POINT('Ctrl Pts',(-0.0545403836274688,-2.1952824096556,
8.12927985626981));
#10726=CARTESIAN_POINT('Ctrl Pts',(-0.0264006657112965,-2.19,8.13));
#10727=CARTESIAN_POINT('Ctrl Pts',(0.0264006657112965,-2.19,8.13));
#10728=CARTESIAN_POINT('Ctrl Pts',(0.0545403836274689,-2.1952824096556,
8.12927985626981));
#10729=CARTESIAN_POINT('Ctrl Pts',(0.106271159541076,-2.21672319916877,
8.12667690933009));
#10730=CARTESIAN_POINT('Ctrl Pts',(0.129864750292352,-2.232879902194,8.12483075953278));
#10731=CARTESIAN_POINT('Ctrl Pts',(0.167120287247804,-2.27013543914945,
8.12135816887013));
#10732=CARTESIAN_POINT('Ctrl Pts',(0.183276841782292,-2.2937289476995,8.11950502964782));
#10733=CARTESIAN_POINT('Ctrl Pts',(0.20471752266132,-2.34545944463489,8.11688606295397));
#10734=CARTESIAN_POINT('Ctrl Pts',(0.21,-2.37359906579625,8.11615888233178));
#10735=CARTESIAN_POINT('Ctrl Pts',(0.21,-2.4,8.11615888233178));
#10736=CARTESIAN_POINT('',(-0.172988438920056,-2.28094119100208,7.52));
#10737=CARTESIAN_POINT('Origin',(0.,-2.4,7.52));
#10738=CARTESIAN_POINT('Ctrl Pts',(0.172988438920056,-2.28094119100209,
7.52));
#10739=CARTESIAN_POINT('Ctrl Pts',(0.165594865311314,-2.27019857760471,
7.52129192197638));
#10740=CARTESIAN_POINT('Ctrl Pts',(0.157297138725606,-2.26031229062726,
7.52265394943905));
#10741=CARTESIAN_POINT('Ctrl Pts',(0.129892073845076,-2.23290722574673,
7.5267480843909));
#10742=CARTESIAN_POINT('Ctrl Pts',(0.106330167759284,-2.21675794366705,
7.52969589327638));
#10743=CARTESIAN_POINT('Ctrl Pts',(0.0546129046324104,-2.19530220603509,
7.53385029472357));
#10744=CARTESIAN_POINT('Ctrl Pts',(0.0264512308298516,-2.19,7.535));
#10745=CARTESIAN_POINT('Ctrl Pts',(-0.0264512308298516,-2.19,7.535));
#10746=CARTESIAN_POINT('Ctrl Pts',(-0.0546129046324104,-2.19530220603509,
7.53385029472357));
#10747=CARTESIAN_POINT('Ctrl Pts',(-0.106330167759284,-2.21675794366705,
7.52969589327638));
#10748=CARTESIAN_POINT('Ctrl Pts',(-0.129892073845076,-2.23290722574673,
7.5267480843909));
#10749=CARTESIAN_POINT('Ctrl Pts',(-0.157297138725606,-2.26031229062726,
7.52265394943905));
#10750=CARTESIAN_POINT('Ctrl Pts',(-0.165594865311315,-2.27019857760471,
7.52129192197638));
#10751=CARTESIAN_POINT('Ctrl Pts',(-0.172988438920056,-2.28094119100208,
7.52));
#10752=CARTESIAN_POINT('Origin',(0.,-2.4,7.52));
#10753=CARTESIAN_POINT('',(-0.172988438920056,-3.6,7.52));
#10754=CARTESIAN_POINT('Origin',(0.,-2.9,6.53));
#10755=CARTESIAN_POINT('',(-1.6,-1.9,6.53));
#10756=CARTESIAN_POINT('Origin',(0.,-1.9,6.53));
#10757=CARTESIAN_POINT('',(-1.6,-2.9,6.53));
#10758=CARTESIAN_POINT('',(-1.6,-2.9,6.53));
#10759=CARTESIAN_POINT('Origin',(0.,-2.9,6.53));
#10760=CARTESIAN_POINT('Origin',(0.,-1.9,6.53));
#10761=CARTESIAN_POINT('',(-1.005,-1.9,6.53));
#10762=CARTESIAN_POINT('Origin',(0.,-1.9,6.53));
#10763=CARTESIAN_POINT('Origin',(0.,-3.6,6.53));
#10764=CARTESIAN_POINT('',(-1.005,-3.5,6.53));
#10765=CARTESIAN_POINT('Origin',(0.,-3.5,6.53));
#10766=CARTESIAN_POINT('',(-1.005,-3.6,6.53));
#10767=CARTESIAN_POINT('Origin',(4.,-3.5,6.53));
#10768=CARTESIAN_POINT('',(4.49999314610979,-3.5,6.52214602235346));
#10769=CARTESIAN_POINT('',(4.,-3.5,6.53));
#10770=CARTESIAN_POINT('',(4.49999314610979,-3.5,6.52214602235346));
#10771=CARTESIAN_POINT('',(4.49999314610979,-2.9,6.52214602235346));
#10772=CARTESIAN_POINT('',(4.49999314610979,-3.5,6.52214602235346));
#10773=CARTESIAN_POINT('',(4.,-2.9,6.53));
#10774=CARTESIAN_POINT('',(4.49999314610979,-2.9,6.52214602235346));
#10775=CARTESIAN_POINT('',(4.,-3.5,6.53));
#10776=CARTESIAN_POINT('Origin',(4.34869235694598,-3.5,7.68709756919613));
#10777=CARTESIAN_POINT('',(4.34869235694598,-3.5,7.68709756919613));
#10778=CARTESIAN_POINT('',(4.,-3.5,6.53));
#10779=CARTESIAN_POINT('',(4.34869235694598,-2.9,7.68709756919613));
#10780=CARTESIAN_POINT('',(4.,-2.9,6.53));
#10781=CARTESIAN_POINT('',(4.34869235694598,-3.5,7.68709756919613));
#10782=CARTESIAN_POINT('Origin',(3.86370330515627,-3.5,7.56527618041008));
#10783=CARTESIAN_POINT('',(3.86370330515627,-3.5,7.56527618041008));
#10784=CARTESIAN_POINT('',(4.34869235694598,-3.5,7.68709756919613));
#10785=CARTESIAN_POINT('',(3.86370330515627,-2.9,7.56527618041008));
#10786=CARTESIAN_POINT('',(4.34869235694598,-2.9,7.68709756919613));
#10787=CARTESIAN_POINT('',(3.86370330515627,-3.5,7.56527618041008));
#10788=CARTESIAN_POINT('Origin',(3.90103537021021,-3.5,8.77319482889224));
#10789=CARTESIAN_POINT('',(3.90103537021021,-3.5,8.77319482889224));
#10790=CARTESIAN_POINT('',(3.86370330515627,-3.5,7.56527618041008));
#10791=CARTESIAN_POINT('',(3.90103537021021,-2.9,8.77319482889224));
#10792=CARTESIAN_POINT('',(3.86370330515627,-2.9,7.56527618041008));
#10793=CARTESIAN_POINT('',(3.90103537021021,-3.5,8.77319482889224));
#10794=CARTESIAN_POINT('Origin',(3.46410161513775,-3.5,8.53));
#10795=CARTESIAN_POINT('',(3.46410161513775,-3.5,8.53));
#10796=CARTESIAN_POINT('',(3.90103537021021,-3.5,8.77319482889224));
#10797=CARTESIAN_POINT('',(3.46410161513775,-2.9,8.53));
#10798=CARTESIAN_POINT('',(3.90103537021021,-2.9,8.77319482889224));
#10799=CARTESIAN_POINT('',(3.46410161513775,-3.5,8.53));
#10800=CARTESIAN_POINT('Origin',(3.18752926976038,-3.5,9.70642206805406));
#10801=CARTESIAN_POINT('',(3.18752926976038,-3.5,9.70642206805406));
#10802=CARTESIAN_POINT('',(3.46410161513775,-3.5,8.53));
#10803=CARTESIAN_POINT('',(3.18752926976038,-2.9,9.70642206805406));
#10804=CARTESIAN_POINT('',(3.46410161513775,-2.9,8.53));
#10805=CARTESIAN_POINT('',(3.18752926976038,-3.5,9.70642206805406));
#10806=CARTESIAN_POINT('Origin',(2.82842712474619,-3.5,9.35842712474619));
#10807=CARTESIAN_POINT('',(2.82842712474619,-3.5,9.35842712474619));
#10808=CARTESIAN_POINT('',(3.18752926976038,-3.5,9.70642206805406));
#10809=CARTESIAN_POINT('',(2.82842712474619,-2.9,9.35842712474619));
#10810=CARTESIAN_POINT('',(3.18752926976038,-2.9,9.70642206805406));
#10811=CARTESIAN_POINT('',(2.82842712474619,-3.5,9.35842712474619));
#10812=CARTESIAN_POINT('Origin',(2.25679831721756,-3.5,10.4231813925637));
#10813=CARTESIAN_POINT('',(2.25679831721756,-3.5,10.4231813925637));
#10814=CARTESIAN_POINT('',(2.82842712474619,-3.5,9.35842712474619));
#10815=CARTESIAN_POINT('',(2.25679831721756,-2.9,10.4231813925637));
#10816=CARTESIAN_POINT('',(2.82842712474619,-2.9,9.35842712474619));
#10817=CARTESIAN_POINT('',(2.25679831721756,-3.5,10.4231813925637));
#10818=CARTESIAN_POINT('Origin',(2.,-3.5,9.99410161513775));
#10819=CARTESIAN_POINT('',(2.,-3.5,9.99410161513775));
#10820=CARTESIAN_POINT('',(2.25679831721756,-3.5,10.4231813925637));
#10821=CARTESIAN_POINT('',(2.,-2.9,9.99410161513775));
#10822=CARTESIAN_POINT('',(2.25679831721756,-2.9,10.4231813925637));
#10823=CARTESIAN_POINT('',(2.,-3.5,9.99410161513775));
#10824=CARTESIAN_POINT('Origin',(1.17227028889192,-3.5,10.8746268389565));
#10825=CARTESIAN_POINT('',(1.17227028889192,-3.5,10.8746268389565));
#10826=CARTESIAN_POINT('',(2.,-3.5,9.99410161513775));
#10827=CARTESIAN_POINT('',(1.17227028889192,-2.9,10.8746268389565));
#10828=CARTESIAN_POINT('',(2.,-2.9,9.99410161513775));
#10829=CARTESIAN_POINT('',(1.17227028889192,-3.5,10.8746268389565));
#10830=CARTESIAN_POINT('Origin',(1.03527618041008,-3.5,10.3937033051563));
#10831=CARTESIAN_POINT('',(1.03527618041008,-3.5,10.3937033051563));
#10832=CARTESIAN_POINT('',(1.17227028889192,-3.5,10.8746268389565));
#10833=CARTESIAN_POINT('',(1.03527618041008,-2.9,10.3937033051563));
#10834=CARTESIAN_POINT('',(1.17227028889192,-2.9,10.8746268389565));
#10835=CARTESIAN_POINT('',(1.03527618041008,-3.5,10.3937033051563));
#10836=CARTESIAN_POINT('Origin',(0.00785397764654228,-3.5,11.0299931461098));
#10837=CARTESIAN_POINT('',(0.00785397764654218,-3.5,11.0299931461098));
#10838=CARTESIAN_POINT('',(1.03527618041008,-3.5,10.3937033051563));
#10839=CARTESIAN_POINT('',(0.00785397764654228,-2.9,11.0299931461098));
#10840=CARTESIAN_POINT('',(1.03527618041008,-2.9,10.3937033051563));
#10841=CARTESIAN_POINT('',(0.00785397764654218,-3.5,11.0299931461098));
#10842=CARTESIAN_POINT('Origin',(2.4459601011273E-16,-3.5,10.53));
#10843=CARTESIAN_POINT('',(2.44929359829471E-16,-3.5,10.53));
#10844=CARTESIAN_POINT('',(0.00785397764654218,-3.5,11.0299931461098));
#10845=CARTESIAN_POINT('',(4.44089209850063E-16,-2.9,10.53));
#10846=CARTESIAN_POINT('',(0.00785397764654218,-2.9,11.0299931461098));
#10847=CARTESIAN_POINT('',(2.44929359829471E-16,-3.5,10.53));
#10848=CARTESIAN_POINT('Origin',(-1.15709756919613,-3.5,10.878692356946));
#10849=CARTESIAN_POINT('',(-1.15709756919613,-3.5,10.878692356946));
#10850=CARTESIAN_POINT('',(2.44929359829471E-16,-3.5,10.53));
#10851=CARTESIAN_POINT('',(-1.15709756919613,-2.9,10.878692356946));
#10852=CARTESIAN_POINT('',(2.44929359829471E-16,-2.9,10.53));
#10853=CARTESIAN_POINT('',(-1.15709756919613,-3.5,10.878692356946));
#10854=CARTESIAN_POINT('Origin',(-1.03527618041008,-3.5,10.3937033051563));
#10855=CARTESIAN_POINT('',(-1.03527618041008,-3.5,10.3937033051563));
#10856=CARTESIAN_POINT('',(-1.15709756919613,-3.5,10.878692356946));
#10857=CARTESIAN_POINT('',(-1.03527618041008,-2.9,10.3937033051563));
#10858=CARTESIAN_POINT('',(-1.15709756919613,-2.9,10.878692356946));
#10859=CARTESIAN_POINT('',(-1.03527618041008,-3.5,10.3937033051563));
#10860=CARTESIAN_POINT('Origin',(-2.24319482889224,-3.5,10.4310353702102));
#10861=CARTESIAN_POINT('',(-2.24319482889224,-3.5,10.4310353702102));
#10862=CARTESIAN_POINT('',(-1.03527618041008,-3.5,10.3937033051563));
#10863=CARTESIAN_POINT('',(-2.24319482889224,-2.9,10.4310353702102));
#10864=CARTESIAN_POINT('',(-1.03527618041008,-2.9,10.3937033051563));
#10865=CARTESIAN_POINT('',(-2.24319482889224,-3.5,10.4310353702102));
#10866=CARTESIAN_POINT('Origin',(-2.,-3.5,9.99410161513775));
#10867=CARTESIAN_POINT('',(-2.,-3.5,9.99410161513775));
#10868=CARTESIAN_POINT('',(-2.24319482889224,-3.5,10.4310353702102));
#10869=CARTESIAN_POINT('',(-2.,-2.9,9.99410161513775));
#10870=CARTESIAN_POINT('',(-2.24319482889224,-2.9,10.4310353702102));
#10871=CARTESIAN_POINT('',(-2.,-3.5,9.99410161513775));
#10872=CARTESIAN_POINT('Origin',(-3.17642206805406,-3.5,9.71752926976038));
#10873=CARTESIAN_POINT('',(-3.17642206805406,-3.5,9.71752926976038));
#10874=CARTESIAN_POINT('',(-2.,-3.5,9.99410161513775));
#10875=CARTESIAN_POINT('',(-3.17642206805406,-2.9,9.71752926976038));
#10876=CARTESIAN_POINT('',(-2.,-2.9,9.99410161513775));
#10877=CARTESIAN_POINT('',(-3.17642206805406,-3.5,9.71752926976038));
#10878=CARTESIAN_POINT('Origin',(-2.82842712474619,-3.5,9.35842712474619));
#10879=CARTESIAN_POINT('',(-2.82842712474619,-3.5,9.35842712474619));
#10880=CARTESIAN_POINT('',(-3.17642206805406,-3.5,9.71752926976038));
#10881=CARTESIAN_POINT('',(-2.82842712474619,-2.9,9.35842712474619));
#10882=CARTESIAN_POINT('',(-3.17642206805406,-2.9,9.71752926976038));
#10883=CARTESIAN_POINT('',(-2.82842712474619,-3.5,9.35842712474619));
#10884=CARTESIAN_POINT('Origin',(-3.89318139256367,-3.5,8.78679831721756));
#10885=CARTESIAN_POINT('',(-3.89318139256367,-3.5,8.78679831721756));
#10886=CARTESIAN_POINT('',(-2.82842712474619,-3.5,9.35842712474619));
#10887=CARTESIAN_POINT('',(-3.89318139256367,-2.9,8.78679831721756));
#10888=CARTESIAN_POINT('',(-2.82842712474619,-2.9,9.35842712474619));
#10889=CARTESIAN_POINT('',(-3.89318139256367,-3.5,8.78679831721756));
#10890=CARTESIAN_POINT('Origin',(-3.46410161513775,-3.5,8.53));
#10891=CARTESIAN_POINT('',(-3.46410161513775,-3.5,8.53));
#10892=CARTESIAN_POINT('',(-3.89318139256367,-3.5,8.78679831721756));
#10893=CARTESIAN_POINT('',(-3.46410161513775,-2.9,8.53));
#10894=CARTESIAN_POINT('',(-3.89318139256367,-2.9,8.78679831721756));
#10895=CARTESIAN_POINT('',(-3.46410161513775,-3.5,8.53));
#10896=CARTESIAN_POINT('Origin',(-4.34462683895651,-3.5,7.70227028889192));
#10897=CARTESIAN_POINT('',(-4.34462683895651,-3.5,7.70227028889192));
#10898=CARTESIAN_POINT('',(-3.46410161513775,-3.5,8.53));
#10899=CARTESIAN_POINT('',(-4.34462683895651,-2.9,7.70227028889192));
#10900=CARTESIAN_POINT('',(-3.46410161513775,-2.9,8.53));
#10901=CARTESIAN_POINT('',(-4.34462683895651,-3.5,7.70227028889192));
#10902=CARTESIAN_POINT('Origin',(-3.86370330515627,-3.5,7.56527618041008));
#10903=CARTESIAN_POINT('',(-3.86370330515627,-3.5,7.56527618041008));
#10904=CARTESIAN_POINT('',(-4.34462683895651,-3.5,7.70227028889192));
#10905=CARTESIAN_POINT('',(-3.86370330515627,-2.9,7.56527618041008));
#10906=CARTESIAN_POINT('',(-4.34462683895651,-2.9,7.70227028889192));
#10907=CARTESIAN_POINT('',(-3.86370330515627,-3.5,7.56527618041008));
#10908=CARTESIAN_POINT('Origin',(-4.49999314610979,-3.5,6.53785397764654));
#10909=CARTESIAN_POINT('',(-4.49999314610979,-3.5,6.53785397764654));
#10910=CARTESIAN_POINT('',(-3.86370330515627,-3.5,7.56527618041008));
#10911=CARTESIAN_POINT('',(-4.49999314610979,-2.9,6.53785397764654));
#10912=CARTESIAN_POINT('',(-3.86370330515627,-2.9,7.56527618041008));
#10913=CARTESIAN_POINT('',(-4.49999314610979,-3.5,6.53785397764654));
#10914=CARTESIAN_POINT('Origin',(-4.,-3.5,6.53));
#10915=CARTESIAN_POINT('',(-4.,-3.5,6.53));
#10916=CARTESIAN_POINT('',(-4.49999314610979,-3.5,6.53785397764654));
#10917=CARTESIAN_POINT('',(-4.,-2.9,6.53));
#10918=CARTESIAN_POINT('',(-4.49999314610979,-2.9,6.53785397764654));
#10919=CARTESIAN_POINT('',(-4.,-3.5,6.53));
#10920=CARTESIAN_POINT('Origin',(-4.34869235694598,-3.5,5.37290243080387));
#10921=CARTESIAN_POINT('',(-4.34869235694598,-3.5,5.37290243080387));
#10922=CARTESIAN_POINT('',(-4.,-3.5,6.53));
#10923=CARTESIAN_POINT('',(-4.34869235694598,-2.9,5.37290243080387));
#10924=CARTESIAN_POINT('',(-4.,-2.9,6.53));
#10925=CARTESIAN_POINT('',(-4.34869235694598,-3.5,5.37290243080387));
#10926=CARTESIAN_POINT('Origin',(-3.86370330515627,-3.5,5.49472381958992));
#10927=CARTESIAN_POINT('',(-3.86370330515627,-3.5,5.49472381958992));
#10928=CARTESIAN_POINT('',(-4.34869235694598,-3.5,5.37290243080387));
#10929=CARTESIAN_POINT('',(-3.86370330515627,-2.9,5.49472381958992));
#10930=CARTESIAN_POINT('',(-4.34869235694598,-2.9,5.37290243080387));
#10931=CARTESIAN_POINT('',(-3.86370330515627,-3.5,5.49472381958992));
#10932=CARTESIAN_POINT('Origin',(-3.90103537021021,-3.5,4.28680517110776));
#10933=CARTESIAN_POINT('',(-3.90103537021021,-3.5,4.28680517110776));
#10934=CARTESIAN_POINT('',(-3.86370330515627,-3.5,5.49472381958992));
#10935=CARTESIAN_POINT('',(-3.90103537021021,-2.9,4.28680517110776));
#10936=CARTESIAN_POINT('',(-3.86370330515627,-2.9,5.49472381958992));
#10937=CARTESIAN_POINT('',(-3.90103537021021,-3.5,4.28680517110776));
#10938=CARTESIAN_POINT('Origin',(-3.46410161513775,-3.5,4.53));
#10939=CARTESIAN_POINT('',(-3.46410161513775,-3.5,4.53));
#10940=CARTESIAN_POINT('',(-3.90103537021021,-3.5,4.28680517110776));
#10941=CARTESIAN_POINT('',(-3.46410161513775,-2.9,4.53));
#10942=CARTESIAN_POINT('',(-3.90103537021021,-2.9,4.28680517110776));
#10943=CARTESIAN_POINT('',(-3.46410161513775,-3.5,4.53));
#10944=CARTESIAN_POINT('Origin',(-3.18752926976038,-3.5,3.35357793194594));
#10945=CARTESIAN_POINT('',(-3.18752926976038,-3.5,3.35357793194594));
#10946=CARTESIAN_POINT('',(-3.46410161513775,-3.5,4.53));
#10947=CARTESIAN_POINT('',(-3.18752926976038,-2.9,3.35357793194594));
#10948=CARTESIAN_POINT('',(-3.46410161513775,-2.9,4.53));
#10949=CARTESIAN_POINT('',(-3.18752926976038,-3.5,3.35357793194594));
#10950=CARTESIAN_POINT('Origin',(-2.82842712474619,-3.5,3.70157287525381));
#10951=CARTESIAN_POINT('',(-2.82842712474619,-3.5,3.70157287525381));
#10952=CARTESIAN_POINT('',(-3.18752926976038,-3.5,3.35357793194594));
#10953=CARTESIAN_POINT('',(-2.82842712474619,-2.9,3.70157287525381));
#10954=CARTESIAN_POINT('',(-3.18752926976038,-2.9,3.35357793194594));
#10955=CARTESIAN_POINT('',(-2.82842712474619,-3.5,3.70157287525381));
#10956=CARTESIAN_POINT('Origin',(-2.25679831721756,-3.5,2.63681860743633));
#10957=CARTESIAN_POINT('',(-2.25679831721756,-3.5,2.63681860743633));
#10958=CARTESIAN_POINT('',(-2.82842712474619,-3.5,3.70157287525381));
#10959=CARTESIAN_POINT('',(-2.25679831721756,-2.9,2.63681860743633));
#10960=CARTESIAN_POINT('',(-2.82842712474619,-2.9,3.70157287525381));
#10961=CARTESIAN_POINT('',(-2.25679831721756,-3.5,2.63681860743633));
#10962=CARTESIAN_POINT('Origin',(-2.,-3.5,3.06589838486225));
#10963=CARTESIAN_POINT('',(-2.,-3.5,3.06589838486225));
#10964=CARTESIAN_POINT('',(-2.25679831721756,-3.5,2.63681860743633));
#10965=CARTESIAN_POINT('',(-2.,-2.9,3.06589838486225));
#10966=CARTESIAN_POINT('',(-2.25679831721756,-2.9,2.63681860743633));
#10967=CARTESIAN_POINT('',(-2.,-3.5,3.06589838486225));
#10968=CARTESIAN_POINT('Origin',(-1.17227028889192,-3.5,2.18537316104349));
#10969=CARTESIAN_POINT('',(-1.17227028889192,-3.5,2.18537316104349));
#10970=CARTESIAN_POINT('',(-2.,-3.5,3.06589838486225));
#10971=CARTESIAN_POINT('',(-1.17227028889192,-2.9,2.18537316104349));
#10972=CARTESIAN_POINT('',(-2.,-2.9,3.06589838486225));
#10973=CARTESIAN_POINT('',(-1.17227028889192,-3.5,2.18537316104349));
#10974=CARTESIAN_POINT('Origin',(-1.03527618041008,-3.5,2.66629669484373));
#10975=CARTESIAN_POINT('',(-1.03527618041008,-3.5,2.66629669484373));
#10976=CARTESIAN_POINT('',(-1.17227028889192,-3.5,2.18537316104349));
#10977=CARTESIAN_POINT('',(-1.03527618041008,-2.9,2.66629669484373));
#10978=CARTESIAN_POINT('',(-1.17227028889192,-2.9,2.18537316104349));
#10979=CARTESIAN_POINT('',(-1.03527618041008,-3.5,2.66629669484373));
#10980=CARTESIAN_POINT('Origin',(-0.00785397764654272,-3.5,2.03000685389021));
#10981=CARTESIAN_POINT('',(-0.00785397764654273,-3.5,2.03000685389021));
#10982=CARTESIAN_POINT('',(-1.03527618041008,-3.5,2.66629669484373));
#10983=CARTESIAN_POINT('',(-0.00785397764654272,-2.9,2.03000685389021));
#10984=CARTESIAN_POINT('',(-1.03527618041008,-2.9,2.66629669484373));
#10985=CARTESIAN_POINT('',(-0.00785397764654273,-3.5,2.03000685389021));
#10986=CARTESIAN_POINT('Origin',(-7.35522753814166E-16,-3.5,2.53));
#10987=CARTESIAN_POINT('',(-7.34788079488412E-16,-3.5,2.53));
#10988=CARTESIAN_POINT('',(-0.00785397764654273,-3.5,2.03000685389021));
#10989=CARTESIAN_POINT('',(-8.88178419700125E-16,-2.9,2.53));
#10990=CARTESIAN_POINT('',(-0.00785397764654273,-2.9,2.03000685389021));
#10991=CARTESIAN_POINT('',(-7.34788079488412E-16,-3.5,2.53));
#10992=CARTESIAN_POINT('Origin',(1.15709756919613,-3.5,2.18130764305402));
#10993=CARTESIAN_POINT('',(1.15709756919613,-3.5,2.18130764305402));
#10994=CARTESIAN_POINT('',(-7.34788079488412E-16,-3.5,2.53));
#10995=CARTESIAN_POINT('',(1.15709756919613,-2.9,2.18130764305402));
#10996=CARTESIAN_POINT('',(-7.34788079488412E-16,-2.9,2.53));
#10997=CARTESIAN_POINT('',(1.15709756919613,-3.5,2.18130764305402));
#10998=CARTESIAN_POINT('Origin',(1.03527618041008,-3.5,2.66629669484373));
#10999=CARTESIAN_POINT('',(1.03527618041008,-3.5,2.66629669484373));
#11000=CARTESIAN_POINT('',(1.15709756919613,-3.5,2.18130764305402));
#11001=CARTESIAN_POINT('',(1.03527618041008,-2.9,2.66629669484373));
#11002=CARTESIAN_POINT('',(1.15709756919613,-2.9,2.18130764305402));
#11003=CARTESIAN_POINT('',(1.03527618041008,-3.5,2.66629669484373));
#11004=CARTESIAN_POINT('Origin',(2.24319482889223,-3.5,2.62896462978979));
#11005=CARTESIAN_POINT('',(2.24319482889223,-3.5,2.62896462978979));
#11006=CARTESIAN_POINT('',(1.03527618041008,-3.5,2.66629669484373));
#11007=CARTESIAN_POINT('',(2.24319482889223,-2.9,2.62896462978979));
#11008=CARTESIAN_POINT('',(1.03527618041008,-2.9,2.66629669484373));
#11009=CARTESIAN_POINT('',(2.24319482889223,-3.5,2.62896462978979));
#11010=CARTESIAN_POINT('Origin',(2.,-3.5,3.06589838486225));
#11011=CARTESIAN_POINT('',(2.,-3.5,3.06589838486225));
#11012=CARTESIAN_POINT('',(2.24319482889223,-3.5,2.62896462978979));
#11013=CARTESIAN_POINT('',(2.,-2.9,3.06589838486225));
#11014=CARTESIAN_POINT('',(2.24319482889223,-2.9,2.62896462978979));
#11015=CARTESIAN_POINT('',(2.,-3.5,3.06589838486225));
#11016=CARTESIAN_POINT('Origin',(3.17642206805406,-3.5,3.34247073023962));
#11017=CARTESIAN_POINT('',(3.17642206805406,-3.5,3.34247073023962));
#11018=CARTESIAN_POINT('',(2.,-3.5,3.06589838486225));
#11019=CARTESIAN_POINT('',(3.17642206805406,-2.9,3.34247073023962));
#11020=CARTESIAN_POINT('',(2.,-2.9,3.06589838486225));
#11021=CARTESIAN_POINT('',(3.17642206805406,-3.5,3.34247073023962));
#11022=CARTESIAN_POINT('Origin',(2.82842712474619,-3.5,3.70157287525381));
#11023=CARTESIAN_POINT('',(2.82842712474619,-3.5,3.70157287525381));
#11024=CARTESIAN_POINT('',(3.17642206805406,-3.5,3.34247073023962));
#11025=CARTESIAN_POINT('',(2.82842712474619,-2.9,3.70157287525381));
#11026=CARTESIAN_POINT('',(3.17642206805406,-2.9,3.34247073023962));
#11027=CARTESIAN_POINT('',(2.82842712474619,-3.5,3.70157287525381));
#11028=CARTESIAN_POINT('Origin',(3.89318139256367,-3.5,4.27320168278244));
#11029=CARTESIAN_POINT('',(3.89318139256367,-3.5,4.27320168278244));
#11030=CARTESIAN_POINT('',(2.82842712474619,-3.5,3.70157287525381));
#11031=CARTESIAN_POINT('',(3.89318139256367,-2.9,4.27320168278244));
#11032=CARTESIAN_POINT('',(2.82842712474619,-2.9,3.70157287525381));
#11033=CARTESIAN_POINT('',(3.89318139256367,-3.5,4.27320168278244));
#11034=CARTESIAN_POINT('Origin',(3.46410161513775,-3.5,4.53));
#11035=CARTESIAN_POINT('',(3.46410161513775,-3.5,4.53));
#11036=CARTESIAN_POINT('',(3.89318139256367,-3.5,4.27320168278244));
#11037=CARTESIAN_POINT('',(3.46410161513775,-2.9,4.53));
#11038=CARTESIAN_POINT('',(3.89318139256367,-2.9,4.27320168278244));
#11039=CARTESIAN_POINT('',(3.46410161513775,-3.5,4.53));
#11040=CARTESIAN_POINT('Origin',(4.34462683895651,-3.5,5.35772971110808));
#11041=CARTESIAN_POINT('',(4.34462683895651,-3.5,5.35772971110808));
#11042=CARTESIAN_POINT('',(3.46410161513775,-3.5,4.53));
#11043=CARTESIAN_POINT('',(4.34462683895651,-2.9,5.35772971110808));
#11044=CARTESIAN_POINT('',(3.46410161513775,-2.9,4.53));
#11045=CARTESIAN_POINT('',(4.34462683895651,-3.5,5.35772971110808));
#11046=CARTESIAN_POINT('Origin',(3.86370330515627,-3.5,5.49472381958992));
#11047=CARTESIAN_POINT('',(3.86370330515627,-3.5,5.49472381958992));
#11048=CARTESIAN_POINT('',(4.34462683895651,-3.5,5.35772971110808));
#11049=CARTESIAN_POINT('',(3.86370330515627,-2.9,5.49472381958992));
#11050=CARTESIAN_POINT('',(4.34462683895651,-2.9,5.35772971110808));
#11051=CARTESIAN_POINT('',(3.86370330515627,-3.5,5.49472381958992));
#11052=CARTESIAN_POINT('Origin',(4.49999314610979,-3.5,6.52214602235346));
#11053=CARTESIAN_POINT('',(3.86370330515627,-3.5,5.49472381958992));
#11054=CARTESIAN_POINT('',(3.86370330515627,-2.9,5.49472381958992));
#11055=CARTESIAN_POINT('Origin',(0.,-2.9,6.53));
#11056=CARTESIAN_POINT('Origin',(0.,-3.5,6.53));
#11057=CARTESIAN_POINT('',(0.,0.,0.));
#11058=CARTESIAN_POINT('Origin',(0.0721687836487032,0.,-0.125));
#11059=CARTESIAN_POINT('',(0.0721687836487032,0.,-0.125));
#11060=CARTESIAN_POINT('',(0.144337567297406,0.,0.));
#11061=CARTESIAN_POINT('',(0.117710979560879,0.,-0.0461186027918559));
#11062=CARTESIAN_POINT('',(0.0721687836487032,-0.25,-0.125));
#11063=CARTESIAN_POINT('',(0.0721687836487032,0.,-0.125));
#11064=CARTESIAN_POINT('',(0.144337567297406,-0.25,0.));
#11065=CARTESIAN_POINT('',(0.144337567297406,-0.25,0.));
#11066=CARTESIAN_POINT('',(0.144337567297406,0.,0.));
#11067=CARTESIAN_POINT('Origin',(-0.0721687836487032,0.,-0.125));
#11068=CARTESIAN_POINT('',(-0.0721687836487032,0.,-0.125));
#11069=CARTESIAN_POINT('',(0.0739156081756484,0.,-0.125));
#11070=CARTESIAN_POINT('',(-0.0721687836487032,-0.25,-0.125));
#11071=CARTESIAN_POINT('',(-0.0721687836487032,0.,-0.125));
#11072=CARTESIAN_POINT('',(0.0721687836487032,-0.25,-0.125));
#11073=CARTESIAN_POINT('Origin',(-0.144337567297406,0.,-4.16333634234434E-17));
#11074=CARTESIAN_POINT('',(-0.144337567297406,0.,-1.76762539787485E-17));
#11075=CARTESIAN_POINT('',(-0.0987953713852306,0.,-0.0788813972081442));
#11076=CARTESIAN_POINT('',(-0.144337567297406,-0.25,-2.77555756156289E-17));
#11077=CARTESIAN_POINT('',(-0.144337567297406,0.,-1.76762539787485E-17));
#11078=CARTESIAN_POINT('',(-0.0721687836487032,-0.25,-0.125));
#11079=CARTESIAN_POINT('Origin',(-0.0721687836487033,0.,0.125));
#11080=CARTESIAN_POINT('',(-0.0721687836487033,0.,0.125));
#11081=CARTESIAN_POINT('',(-0.0627109795608791,0.,0.141381397208144));
#11082=CARTESIAN_POINT('',(-0.0721687836487033,-0.25,0.125));
#11083=CARTESIAN_POINT('',(-0.0721687836487033,0.,0.125));
#11084=CARTESIAN_POINT('',(-0.144337567297406,-0.25,-1.76762539787485E-17));
#11085=CARTESIAN_POINT('Origin',(0.0721687836487032,0.,0.125));
#11086=CARTESIAN_POINT('',(0.0721687836487032,0.,0.125));
#11087=CARTESIAN_POINT('',(0.146084391824352,0.,0.125));
#11088=CARTESIAN_POINT('',(0.0721687836487032,-0.25,0.125));
#11089=CARTESIAN_POINT('',(0.0721687836487032,0.,0.125));
#11090=CARTESIAN_POINT('',(-0.0721687836487033,-0.25,0.125));
#11091=CARTESIAN_POINT('Origin',(0.144337567297406,0.,0.));
#11092=CARTESIAN_POINT('',(0.153795371385231,0.,-0.0163813972081441));
#11093=CARTESIAN_POINT('',(0.0721687836487032,-0.25,0.125));
#11094=CARTESIAN_POINT('Origin',(0.,-0.25,0.));
#11095=CARTESIAN_POINT('Origin',(0.22,0.,0.));
#11096=CARTESIAN_POINT('',(-0.22,-8.67361737988404E-18,-2.69422295812418E-17));
#11097=CARTESIAN_POINT('Origin',(0.,0.,0.));
#11098=CARTESIAN_POINT('Origin',(0.,-0.015,0.));
#11099=CARTESIAN_POINT('',(-0.24505,-0.02505,-3.00099698131059E-17));
#11100=CARTESIAN_POINT('Origin',(0.,-0.02505,0.));
#11101=CARTESIAN_POINT('',(-0.235,-0.015,-2.87791997799628E-17));
#11102=CARTESIAN_POINT('Origin',(0.,-0.3775,0.));
#11103=CARTESIAN_POINT('',(-0.24505,-0.72995,3.00099698131059E-17));
#11104=CARTESIAN_POINT('Origin',(0.,-0.72995,0.));
#11105=CARTESIAN_POINT('',(-0.24505,-0.3775,-3.00099698131059E-17));
#11106=CARTESIAN_POINT('Origin',(0.,-0.7625,0.));
#11107=CARTESIAN_POINT('',(-0.175,-0.8,-2.14313189850787E-17));
#11108=CARTESIAN_POINT('Origin',(0.,-0.8,0.));
#11109=CARTESIAN_POINT('',(-0.2125,-0.7625,-2.60237444818813E-17));
#11110=CARTESIAN_POINT('Origin',(0.,-0.8,0.));
#11111=CARTESIAN_POINT('',(0.,0.,0.));
#11112=CARTESIAN_POINT('',(0.,0.,0.));
#11113=CARTESIAN_POINT('',(0.,0.,0.));
#11114=CARTESIAN_POINT('',(0.9,0.,1.4));
#11115=CARTESIAN_POINT('',(0.,6.53,8.3));
#11116=CARTESIAN_POINT('',(0.,-1.8,5.9));
#11117=CARTESIAN_POINT('',(0.,0.,0.));
#11118=CARTESIAN_POINT('',(0.,0.,0.));
#11119=CARTESIAN_POINT('Origin',(6.5,-3.47,5.4));
#11120=CARTESIAN_POINT('',(6.93208101356604,-3.19906458755684,5.52));
#11121=CARTESIAN_POINT('',(6.93208101356604,-3.19906458755684,5.4));
#11122=CARTESIAN_POINT('',(6.93208101356604,-3.19906458755684,5.4));
#11123=CARTESIAN_POINT('',(6.44729373923199,-2.96273079131899,5.52));
#11124=CARTESIAN_POINT('Origin',(6.5,-3.47,5.52));
#11125=CARTESIAN_POINT('',(6.44729373923199,-2.96273079131899,5.4));
#11126=CARTESIAN_POINT('',(6.44729373923199,-2.96273079131899,5.4));
#11127=CARTESIAN_POINT('Origin',(6.5,-3.47,5.4));
#11128=CARTESIAN_POINT('Origin',(5.6,-1.935,5.4));
#11129=CARTESIAN_POINT('',(6.627369839284,-2.59334391941745,5.4));
#11130=CARTESIAN_POINT('',(6.83470395152127,-2.16804317636662,5.4));
#11131=CARTESIAN_POINT('',(4.6,-8.88178419700125E-16,5.4));
#11132=CARTESIAN_POINT('',(4.6,-8.88178419700125E-16,5.4));
#11133=CARTESIAN_POINT('',(4.2,-8.88178419700125E-16,5.4));
#11134=CARTESIAN_POINT('',(4.2,-8.88178419700125E-16,5.4));
#11135=CARTESIAN_POINT('',(5.96787188180707,-3.01520370952651,5.4));
#11136=CARTESIAN_POINT('',(6.,-3.07,5.4));
#11137=CARTESIAN_POINT('',(7.02546072606318,-3.00751645935757,5.4));
#11138=CARTESIAN_POINT('Origin',(6.5,-3.47,5.4));
#11139=CARTESIAN_POINT('',(6.9870975886883,-3.08621007448555,5.4));
#11140=CARTESIAN_POINT('',(6.195,-3.47,5.4));
#11141=CARTESIAN_POINT('Origin',(6.5,-3.47,5.4));
#11142=CARTESIAN_POINT('Origin',(7.28,-1.87,5.52));
#11143=CARTESIAN_POINT('',(7.18,-1.87,5.88));
#11144=CARTESIAN_POINT('Origin',(7.28,-1.87,5.88));
#11145=CARTESIAN_POINT('',(7.18,-1.87,5.52));
#11146=CARTESIAN_POINT('',(7.18,-1.87,5.52));
#11147=CARTESIAN_POINT('',(7.38,-1.87,5.52));
#11148=CARTESIAN_POINT('Origin',(7.28,-1.87,5.52));
#11149=CARTESIAN_POINT('Origin',(7.28,-1.87,5.52));
#11150=CARTESIAN_POINT('Origin',(7.28,-1.87,5.88));
#11151=CARTESIAN_POINT('Origin',(7.28,-1.87,5.52));
#11152=CARTESIAN_POINT('',(7.58,-1.87,5.52));
#11153=CARTESIAN_POINT('Origin',(6.89,-2.67,5.4));
#11154=CARTESIAN_POINT('',(6.83016839641497,-2.85275707374749,5.4));
#11155=CARTESIAN_POINT('Origin',(6.5,-3.47,5.4));
#11156=CARTESIAN_POINT('',(4.6,-8.88178419700125E-16,5.4));
#11157=CARTESIAN_POINT('',(6.98,-1.87,5.4));
#11158=CARTESIAN_POINT('',(6.98,-1.87,5.4));
#11159=CARTESIAN_POINT('',(7.58,-1.87,5.4));
#11160=CARTESIAN_POINT('',(7.58,-1.87,5.4));
#11161=CARTESIAN_POINT('',(6.8,-3.47,5.4));
#11162=CARTESIAN_POINT('Origin',(7.58,-1.87,5.4));
#11163=CARTESIAN_POINT('',(6.98,-1.87,5.52));
#11164=CARTESIAN_POINT('',(6.98,-1.87,5.4));
#11165=CARTESIAN_POINT('',(7.58,-1.87,5.52));
#11166=CARTESIAN_POINT('',(7.58,-1.87,5.52));
#11167=CARTESIAN_POINT('',(7.58,-1.87,5.52));
#11168=CARTESIAN_POINT('',(7.58,-1.87,5.4));
#11169=CARTESIAN_POINT('Origin',(6.8,-3.47,5.4));
#11170=CARTESIAN_POINT('',(6.8,-3.47,5.52));
#11171=CARTESIAN_POINT('Origin',(6.98,-1.87,5.4));
#11172=CARTESIAN_POINT('',(6.98,-1.87,5.52));
#11173=CARTESIAN_POINT('Origin',(6.89,-2.67,5.52));
#11174=CARTESIAN_POINT('Origin',(6.5,-3.47,4.7));
#11175=CARTESIAN_POINT('',(6.195,-3.47,4.8));
#11176=CARTESIAN_POINT('Origin',(6.5,-3.47,4.8));
#11177=CARTESIAN_POINT('',(6.195,-3.47,4.7));
#11178=CARTESIAN_POINT('Origin',(6.5,-3.47,4.8));
#11179=CARTESIAN_POINT('',(5.96787188180707,-3.01520370952651,4.8));
#11180=CARTESIAN_POINT('',(5.96787188180707,-3.01520370952651,4.8));
#11181=CARTESIAN_POINT('',(6.83016839641497,-2.85275707374749,4.8));
#11182=CARTESIAN_POINT('Origin',(6.5,-3.47,4.8));
#11183=CARTESIAN_POINT('',(6.83016839641497,-2.85275707374749,4.8));
#11184=CARTESIAN_POINT('Origin',(4.2,-8.88178419700125E-16,4.8));
#11185=CARTESIAN_POINT('',(4.2,-8.88178419700125E-16,4.8));
#11186=CARTESIAN_POINT('',(4.2,-8.88178419700125E-16,4.8));
#11187=CARTESIAN_POINT('',(6.,-3.07,4.8));
#11188=CARTESIAN_POINT('Origin',(4.6,-8.88178419700125E-16,4.8));
#11189=CARTESIAN_POINT('',(4.6,-8.88178419700125E-16,4.8));
#11190=CARTESIAN_POINT('',(4.2,-8.88178419700125E-16,4.8));
#11191=CARTESIAN_POINT('',(4.6,-8.88178419700125E-16,4.8));
#11192=CARTESIAN_POINT('Origin',(7.,-3.07,4.8));
#11193=CARTESIAN_POINT('',(4.6,-8.88178419700125E-16,4.8));
#11194=CARTESIAN_POINT('Origin',(5.6,-1.935,4.8));
#11195=CARTESIAN_POINT('',(0.,0.,0.));
#11196=CARTESIAN_POINT('',(0.,0.,0.));
#11197=CARTESIAN_POINT('',(-2.36387745779394E-17,-2.60236526666083E-16,
0.));
#11198=CARTESIAN_POINT('',(5.82867087928207E-15,-4.44089209850063E-15,-1.56514286095996E-15));
#11199=UNCERTAINTY_MEASURE_WITH_UNIT(LENGTH_MEASURE(0.001),#11259,
'DISTANCE_ACCURACY_VALUE',
'Maximum model space distance between geometric entities at asserted c
onnectivities');
#11200=UNCERTAINTY_MEASURE_WITH_UNIT(LENGTH_MEASURE(0.001),#11259,
'DISTANCE_ACCURACY_VALUE',
'Maximum model space distance between geometric entities at asserted c
onnectivities');
#11201=UNCERTAINTY_MEASURE_WITH_UNIT(LENGTH_MEASURE(0.001),#11259,
'DISTANCE_ACCURACY_VALUE',
'Maximum model space distance between geometric entities at asserted c
onnectivities');
#11202=UNCERTAINTY_MEASURE_WITH_UNIT(LENGTH_MEASURE(0.001),#11259,
'DISTANCE_ACCURACY_VALUE',
'Maximum model space distance between geometric entities at asserted c
onnectivities');
#11203=UNCERTAINTY_MEASURE_WITH_UNIT(LENGTH_MEASURE(0.001),#11259,
'DISTANCE_ACCURACY_VALUE',
'Maximum model space distance between geometric entities at asserted c
onnectivities');
#11204=UNCERTAINTY_MEASURE_WITH_UNIT(LENGTH_MEASURE(0.001),#11259,
'DISTANCE_ACCURACY_VALUE',
'Maximum model space distance between geometric entities at asserted c
onnectivities');
#11205=UNCERTAINTY_MEASURE_WITH_UNIT(LENGTH_MEASURE(0.001),#11259,
'DISTANCE_ACCURACY_VALUE',
'Maximum model space distance between geometric entities at asserted c
onnectivities');
#11206=UNCERTAINTY_MEASURE_WITH_UNIT(LENGTH_MEASURE(0.001),#11259,
'DISTANCE_ACCURACY_VALUE',
'Maximum model space distance between geometric entities at asserted c
onnectivities');
#11207=UNCERTAINTY_MEASURE_WITH_UNIT(LENGTH_MEASURE(0.001),#11259,
'DISTANCE_ACCURACY_VALUE',
'Maximum model space distance between geometric entities at asserted c
onnectivities');
#11208=UNCERTAINTY_MEASURE_WITH_UNIT(LENGTH_MEASURE(0.001),#11259,
'DISTANCE_ACCURACY_VALUE',
'Maximum model space distance between geometric entities at asserted c
onnectivities');
#11209=UNCERTAINTY_MEASURE_WITH_UNIT(LENGTH_MEASURE(0.001),#11259,
'DISTANCE_ACCURACY_VALUE',
'Maximum model space distance between geometric entities at asserted c
onnectivities');
#11210=UNCERTAINTY_MEASURE_WITH_UNIT(LENGTH_MEASURE(0.001),#11259,
'DISTANCE_ACCURACY_VALUE',
'Maximum model space distance between geometric entities at asserted c
onnectivities');
#11211=UNCERTAINTY_MEASURE_WITH_UNIT(LENGTH_MEASURE(0.001),#11259,
'DISTANCE_ACCURACY_VALUE',
'Maximum model space distance between geometric entities at asserted c
onnectivities');
#11212=UNCERTAINTY_MEASURE_WITH_UNIT(LENGTH_MEASURE(0.001),#11259,
'DISTANCE_ACCURACY_VALUE',
'Maximum model space distance between geometric entities at asserted c
onnectivities');
#11213=UNCERTAINTY_MEASURE_WITH_UNIT(LENGTH_MEASURE(0.001),#11259,
'DISTANCE_ACCURACY_VALUE',
'Maximum model space distance between geometric entities at asserted c
onnectivities');
#11214=UNCERTAINTY_MEASURE_WITH_UNIT(LENGTH_MEASURE(0.001),#11259,
'DISTANCE_ACCURACY_VALUE',
'Maximum model space distance between geometric entities at asserted c
onnectivities');
#11215=UNCERTAINTY_MEASURE_WITH_UNIT(LENGTH_MEASURE(0.001),#11259,
'DISTANCE_ACCURACY_VALUE',
'Maximum model space distance between geometric entities at asserted c
onnectivities');
#11216=UNCERTAINTY_MEASURE_WITH_UNIT(LENGTH_MEASURE(0.001),#11259,
'DISTANCE_ACCURACY_VALUE',
'Maximum model space distance between geometric entities at asserted c
onnectivities');
#11217=UNCERTAINTY_MEASURE_WITH_UNIT(LENGTH_MEASURE(0.001),#11259,
'DISTANCE_ACCURACY_VALUE',
'Maximum model space distance between geometric entities at asserted c
onnectivities');
#11218=UNCERTAINTY_MEASURE_WITH_UNIT(LENGTH_MEASURE(0.001),#11259,
'DISTANCE_ACCURACY_VALUE',
'Maximum model space distance between geometric entities at asserted c
onnectivities');
#11219=UNCERTAINTY_MEASURE_WITH_UNIT(LENGTH_MEASURE(0.001),#11259,
'DISTANCE_ACCURACY_VALUE',
'Maximum model space distance between geometric entities at asserted c
onnectivities');
#11220=UNCERTAINTY_MEASURE_WITH_UNIT(LENGTH_MEASURE(0.001),#11259,
'DISTANCE_ACCURACY_VALUE',
'Maximum model space distance between geometric entities at asserted c
onnectivities');
#11221=UNCERTAINTY_MEASURE_WITH_UNIT(LENGTH_MEASURE(0.001),#11259,
'DISTANCE_ACCURACY_VALUE',
'Maximum model space distance between geometric entities at asserted c
onnectivities');
#11222=UNCERTAINTY_MEASURE_WITH_UNIT(LENGTH_MEASURE(0.001),#11259,
'DISTANCE_ACCURACY_VALUE',
'Maximum model space distance between geometric entities at asserted c
onnectivities');
#11223=UNCERTAINTY_MEASURE_WITH_UNIT(LENGTH_MEASURE(0.001),#11259,
'DISTANCE_ACCURACY_VALUE',
'Maximum model space distance between geometric entities at asserted c
onnectivities');
#11224=UNCERTAINTY_MEASURE_WITH_UNIT(LENGTH_MEASURE(0.001),#11259,
'DISTANCE_ACCURACY_VALUE',
'Maximum model space distance between geometric entities at asserted c
onnectivities');
#11225=UNCERTAINTY_MEASURE_WITH_UNIT(LENGTH_MEASURE(0.001),#11259,
'DISTANCE_ACCURACY_VALUE',
'Maximum model space distance between geometric entities at asserted c
onnectivities');
#11226=UNCERTAINTY_MEASURE_WITH_UNIT(LENGTH_MEASURE(0.001),#11259,
'DISTANCE_ACCURACY_VALUE',
'Maximum model space distance between geometric entities at asserted c
onnectivities');
#11227=UNCERTAINTY_MEASURE_WITH_UNIT(LENGTH_MEASURE(0.001),#11259,
'DISTANCE_ACCURACY_VALUE',
'Maximum model space distance between geometric entities at asserted c
onnectivities');
#11228=UNCERTAINTY_MEASURE_WITH_UNIT(LENGTH_MEASURE(0.001),#11259,
'DISTANCE_ACCURACY_VALUE',
'Maximum model space distance between geometric entities at asserted c
onnectivities');
#11229=(
GEOMETRIC_REPRESENTATION_CONTEXT(3)
GLOBAL_UNCERTAINTY_ASSIGNED_CONTEXT((#11199))
GLOBAL_UNIT_ASSIGNED_CONTEXT((#11259,#11261,#11262))
REPRESENTATION_CONTEXT('','3D')
);
#11230=(
GEOMETRIC_REPRESENTATION_CONTEXT(3)
GLOBAL_UNCERTAINTY_ASSIGNED_CONTEXT((#11200))
GLOBAL_UNIT_ASSIGNED_CONTEXT((#11259,#11261,#11262))
REPRESENTATION_CONTEXT('','3D')
);
#11231=(
GEOMETRIC_REPRESENTATION_CONTEXT(3)
GLOBAL_UNCERTAINTY_ASSIGNED_CONTEXT((#11201))
GLOBAL_UNIT_ASSIGNED_CONTEXT((#11259,#11261,#11262))
REPRESENTATION_CONTEXT('','3D')
);
#11232=(
GEOMETRIC_REPRESENTATION_CONTEXT(3)
GLOBAL_UNCERTAINTY_ASSIGNED_CONTEXT((#11202))
GLOBAL_UNIT_ASSIGNED_CONTEXT((#11259,#11261,#11262))
REPRESENTATION_CONTEXT('','3D')
);
#11233=(
GEOMETRIC_REPRESENTATION_CONTEXT(3)
GLOBAL_UNCERTAINTY_ASSIGNED_CONTEXT((#11203))
GLOBAL_UNIT_ASSIGNED_CONTEXT((#11259,#11261,#11262))
REPRESENTATION_CONTEXT('','3D')
);
#11234=(
GEOMETRIC_REPRESENTATION_CONTEXT(3)
GLOBAL_UNCERTAINTY_ASSIGNED_CONTEXT((#11204))
GLOBAL_UNIT_ASSIGNED_CONTEXT((#11259,#11261,#11262))
REPRESENTATION_CONTEXT('','3D')
);
#11235=(
GEOMETRIC_REPRESENTATION_CONTEXT(3)
GLOBAL_UNCERTAINTY_ASSIGNED_CONTEXT((#11205))
GLOBAL_UNIT_ASSIGNED_CONTEXT((#11259,#11261,#11262))
REPRESENTATION_CONTEXT('','3D')
);
#11236=(
GEOMETRIC_REPRESENTATION_CONTEXT(3)
GLOBAL_UNCERTAINTY_ASSIGNED_CONTEXT((#11206))
GLOBAL_UNIT_ASSIGNED_CONTEXT((#11259,#11261,#11262))
REPRESENTATION_CONTEXT('','3D')
);
#11237=(
GEOMETRIC_REPRESENTATION_CONTEXT(3)
GLOBAL_UNCERTAINTY_ASSIGNED_CONTEXT((#11207))
GLOBAL_UNIT_ASSIGNED_CONTEXT((#11259,#11261,#11262))
REPRESENTATION_CONTEXT('','3D')
);
#11238=(
GEOMETRIC_REPRESENTATION_CONTEXT(3)
GLOBAL_UNCERTAINTY_ASSIGNED_CONTEXT((#11208))
GLOBAL_UNIT_ASSIGNED_CONTEXT((#11259,#11261,#11262))
REPRESENTATION_CONTEXT('','3D')
);
#11239=(
GEOMETRIC_REPRESENTATION_CONTEXT(3)
GLOBAL_UNCERTAINTY_ASSIGNED_CONTEXT((#11209))
GLOBAL_UNIT_ASSIGNED_CONTEXT((#11259,#11261,#11262))
REPRESENTATION_CONTEXT('','3D')
);
#11240=(
GEOMETRIC_REPRESENTATION_CONTEXT(3)
GLOBAL_UNCERTAINTY_ASSIGNED_CONTEXT((#11210))
GLOBAL_UNIT_ASSIGNED_CONTEXT((#11259,#11261,#11262))
REPRESENTATION_CONTEXT('','3D')
);
#11241=(
GEOMETRIC_REPRESENTATION_CONTEXT(3)
GLOBAL_UNCERTAINTY_ASSIGNED_CONTEXT((#11211))
GLOBAL_UNIT_ASSIGNED_CONTEXT((#11259,#11261,#11262))
REPRESENTATION_CONTEXT('','3D')
);
#11242=(
GEOMETRIC_REPRESENTATION_CONTEXT(3)
GLOBAL_UNCERTAINTY_ASSIGNED_CONTEXT((#11212))
GLOBAL_UNIT_ASSIGNED_CONTEXT((#11259,#11261,#11262))
REPRESENTATION_CONTEXT('','3D')
);
#11243=(
GEOMETRIC_REPRESENTATION_CONTEXT(3)
GLOBAL_UNCERTAINTY_ASSIGNED_CONTEXT((#11213))
GLOBAL_UNIT_ASSIGNED_CONTEXT((#11259,#11261,#11262))
REPRESENTATION_CONTEXT('','3D')
);
#11244=(
GEOMETRIC_REPRESENTATION_CONTEXT(3)
GLOBAL_UNCERTAINTY_ASSIGNED_CONTEXT((#11214))
GLOBAL_UNIT_ASSIGNED_CONTEXT((#11259,#11261,#11262))
REPRESENTATION_CONTEXT('','3D')
);
#11245=(
GEOMETRIC_REPRESENTATION_CONTEXT(3)
GLOBAL_UNCERTAINTY_ASSIGNED_CONTEXT((#11215))
GLOBAL_UNIT_ASSIGNED_CONTEXT((#11259,#11261,#11262))
REPRESENTATION_CONTEXT('','3D')
);
#11246=(
GEOMETRIC_REPRESENTATION_CONTEXT(3)
GLOBAL_UNCERTAINTY_ASSIGNED_CONTEXT((#11216))
GLOBAL_UNIT_ASSIGNED_CONTEXT((#11259,#11261,#11262))
REPRESENTATION_CONTEXT('','3D')
);
#11247=(
GEOMETRIC_REPRESENTATION_CONTEXT(3)
GLOBAL_UNCERTAINTY_ASSIGNED_CONTEXT((#11217))
GLOBAL_UNIT_ASSIGNED_CONTEXT((#11259,#11261,#11262))
REPRESENTATION_CONTEXT('','3D')
);
#11248=(
GEOMETRIC_REPRESENTATION_CONTEXT(3)
GLOBAL_UNCERTAINTY_ASSIGNED_CONTEXT((#11218))
GLOBAL_UNIT_ASSIGNED_CONTEXT((#11259,#11261,#11262))
REPRESENTATION_CONTEXT('','3D')
);
#11249=(
GEOMETRIC_REPRESENTATION_CONTEXT(3)
GLOBAL_UNCERTAINTY_ASSIGNED_CONTEXT((#11219))
GLOBAL_UNIT_ASSIGNED_CONTEXT((#11259,#11261,#11262))
REPRESENTATION_CONTEXT('','3D')
);
#11250=(
GEOMETRIC_REPRESENTATION_CONTEXT(3)
GLOBAL_UNCERTAINTY_ASSIGNED_CONTEXT((#11220))
GLOBAL_UNIT_ASSIGNED_CONTEXT((#11259,#11261,#11262))
REPRESENTATION_CONTEXT('','3D')
);
#11251=(
GEOMETRIC_REPRESENTATION_CONTEXT(3)
GLOBAL_UNCERTAINTY_ASSIGNED_CONTEXT((#11221))
GLOBAL_UNIT_ASSIGNED_CONTEXT((#11259,#11261,#11262))
REPRESENTATION_CONTEXT('','3D')
);
#11252=(
GEOMETRIC_REPRESENTATION_CONTEXT(3)
GLOBAL_UNCERTAINTY_ASSIGNED_CONTEXT((#11222))
GLOBAL_UNIT_ASSIGNED_CONTEXT((#11259,#11261,#11262))
REPRESENTATION_CONTEXT('','3D')
);
#11253=(
GEOMETRIC_REPRESENTATION_CONTEXT(3)
GLOBAL_UNCERTAINTY_ASSIGNED_CONTEXT((#11223))
GLOBAL_UNIT_ASSIGNED_CONTEXT((#11259,#11261,#11262))
REPRESENTATION_CONTEXT('','3D')
);
#11254=(
GEOMETRIC_REPRESENTATION_CONTEXT(3)
GLOBAL_UNCERTAINTY_ASSIGNED_CONTEXT((#11224))
GLOBAL_UNIT_ASSIGNED_CONTEXT((#11259,#11261,#11262))
REPRESENTATION_CONTEXT('','3D')
);
#11255=(
GEOMETRIC_REPRESENTATION_CONTEXT(3)
GLOBAL_UNCERTAINTY_ASSIGNED_CONTEXT((#11225))
GLOBAL_UNIT_ASSIGNED_CONTEXT((#11259,#11261,#11262))
REPRESENTATION_CONTEXT('','3D')
);
#11256=(
GEOMETRIC_REPRESENTATION_CONTEXT(3)
GLOBAL_UNCERTAINTY_ASSIGNED_CONTEXT((#11226))
GLOBAL_UNIT_ASSIGNED_CONTEXT((#11259,#11261,#11262))
REPRESENTATION_CONTEXT('','3D')
);
#11257=(
GEOMETRIC_REPRESENTATION_CONTEXT(3)
GLOBAL_UNCERTAINTY_ASSIGNED_CONTEXT((#11227))
GLOBAL_UNIT_ASSIGNED_CONTEXT((#11259,#11261,#11262))
REPRESENTATION_CONTEXT('','3D')
);
#11258=(
GEOMETRIC_REPRESENTATION_CONTEXT(3)
GLOBAL_UNCERTAINTY_ASSIGNED_CONTEXT((#11228))
GLOBAL_UNIT_ASSIGNED_CONTEXT((#11259,#11261,#11262))
REPRESENTATION_CONTEXT('','3D')
);
#11259=(
LENGTH_UNIT()
NAMED_UNIT(*)
SI_UNIT(.CENTI.,.METRE.)
);
#11260=(
LENGTH_UNIT()
NAMED_UNIT(*)
SI_UNIT($,.METRE.)
);
#11261=(
NAMED_UNIT(*)
PLANE_ANGLE_UNIT()
SI_UNIT($,.RADIAN.)
);
#11262=(
NAMED_UNIT(*)
SI_UNIT($,.STERADIAN.)
SOLID_ANGLE_UNIT()
);
#11263=SHAPE_DEFINITION_REPRESENTATION(#11292,#11359);
#11264=SHAPE_DEFINITION_REPRESENTATION(#11293,#11360);
#11265=SHAPE_DEFINITION_REPRESENTATION(#11294,#11361);
#11266=SHAPE_DEFINITION_REPRESENTATION(#11295,#11362);
#11267=SHAPE_DEFINITION_REPRESENTATION(#11296,#11363);
#11268=SHAPE_DEFINITION_REPRESENTATION(#11297,#11364);
#11269=SHAPE_DEFINITION_REPRESENTATION(#11298,#11365);
#11270=SHAPE_DEFINITION_REPRESENTATION(#11299,#11366);
#11271=SHAPE_DEFINITION_REPRESENTATION(#11300,#11367);
#11272=SHAPE_DEFINITION_REPRESENTATION(#11301,#11368);
#11273=SHAPE_DEFINITION_REPRESENTATION(#11302,#11369);
#11274=SHAPE_DEFINITION_REPRESENTATION(#11303,#11370);
#11275=SHAPE_DEFINITION_REPRESENTATION(#11304,#11371);
#11276=SHAPE_DEFINITION_REPRESENTATION(#11305,#11372);
#11277=SHAPE_DEFINITION_REPRESENTATION(#11306,#11373);
#11278=SHAPE_DEFINITION_REPRESENTATION(#11307,#11374);
#11279=SHAPE_DEFINITION_REPRESENTATION(#11308,#11375);
#11280=SHAPE_DEFINITION_REPRESENTATION(#11314,#11376);
#11281=SHAPE_DEFINITION_REPRESENTATION(#11315,#11377);
#11282=SHAPE_DEFINITION_REPRESENTATION(#11316,#11378);
#11283=SHAPE_DEFINITION_REPRESENTATION(#11340,#11379);
#11284=SHAPE_DEFINITION_REPRESENTATION(#11341,#11380);
#11285=SHAPE_DEFINITION_REPRESENTATION(#11342,#11381);
#11286=SHAPE_DEFINITION_REPRESENTATION(#11343,#11382);
#11287=SHAPE_DEFINITION_REPRESENTATION(#11344,#11383);
#11288=SHAPE_DEFINITION_REPRESENTATION(#11345,#11384);
#11289=SHAPE_DEFINITION_REPRESENTATION(#11346,#11385);
#11290=SHAPE_DEFINITION_REPRESENTATION(#11353,#11386);
#11291=SHAPE_DEFINITION_REPRESENTATION(#11354,#11387);
#11292=PRODUCT_DEFINITION_SHAPE('',$,#11389);
#11293=PRODUCT_DEFINITION_SHAPE('',$,#11390);
#11294=PRODUCT_DEFINITION_SHAPE('',$,#11391);
#11295=PRODUCT_DEFINITION_SHAPE('',$,#11392);
#11296=PRODUCT_DEFINITION_SHAPE('',$,#11393);
#11297=PRODUCT_DEFINITION_SHAPE('',$,#11394);
#11298=PRODUCT_DEFINITION_SHAPE('',$,#11395);
#11299=PRODUCT_DEFINITION_SHAPE('',$,#11396);
#11300=PRODUCT_DEFINITION_SHAPE('',$,#11397);
#11301=PRODUCT_DEFINITION_SHAPE('',$,#11398);
#11302=PRODUCT_DEFINITION_SHAPE('',$,#11399);
#11303=PRODUCT_DEFINITION_SHAPE('',$,#11400);
#11304=PRODUCT_DEFINITION_SHAPE('',$,#11401);
#11305=PRODUCT_DEFINITION_SHAPE('',$,#11402);
#11306=PRODUCT_DEFINITION_SHAPE('',$,#11403);
#11307=PRODUCT_DEFINITION_SHAPE('',$,#11404);
#11308=PRODUCT_DEFINITION_SHAPE('',$,#11405);
#11309=PRODUCT_DEFINITION_SHAPE($,$,#132);
#11310=PRODUCT_DEFINITION_SHAPE($,$,#133);
#11311=PRODUCT_DEFINITION_SHAPE($,$,#134);
#11312=PRODUCT_DEFINITION_SHAPE($,$,#135);
#11313=PRODUCT_DEFINITION_SHAPE($,$,#136);
#11314=PRODUCT_DEFINITION_SHAPE('',$,#11406);
#11315=PRODUCT_DEFINITION_SHAPE('',$,#11407);
#11316=PRODUCT_DEFINITION_SHAPE('',$,#11408);
#11317=PRODUCT_DEFINITION_SHAPE($,$,#137);
#11318=PRODUCT_DEFINITION_SHAPE($,$,#138);
#11319=PRODUCT_DEFINITION_SHAPE($,$,#139);
#11320=PRODUCT_DEFINITION_SHAPE($,$,#140);
#11321=PRODUCT_DEFINITION_SHAPE($,$,#141);
#11322=PRODUCT_DEFINITION_SHAPE($,$,#142);
#11323=PRODUCT_DEFINITION_SHAPE($,$,#143);
#11324=PRODUCT_DEFINITION_SHAPE($,$,#144);
#11325=PRODUCT_DEFINITION_SHAPE($,$,#145);
#11326=PRODUCT_DEFINITION_SHAPE($,$,#146);
#11327=PRODUCT_DEFINITION_SHAPE($,$,#147);
#11328=PRODUCT_DEFINITION_SHAPE($,$,#148);
#11329=PRODUCT_DEFINITION_SHAPE($,$,#149);
#11330=PRODUCT_DEFINITION_SHAPE($,$,#150);
#11331=PRODUCT_DEFINITION_SHAPE($,$,#151);
#11332=PRODUCT_DEFINITION_SHAPE($,$,#152);
#11333=PRODUCT_DEFINITION_SHAPE($,$,#153);
#11334=PRODUCT_DEFINITION_SHAPE($,$,#154);
#11335=PRODUCT_DEFINITION_SHAPE($,$,#155);
#11336=PRODUCT_DEFINITION_SHAPE($,$,#156);
#11337=PRODUCT_DEFINITION_SHAPE($,$,#157);
#11338=PRODUCT_DEFINITION_SHAPE($,$,#158);
#11339=PRODUCT_DEFINITION_SHAPE($,$,#159);
#11340=PRODUCT_DEFINITION_SHAPE('',$,#11409);
#11341=PRODUCT_DEFINITION_SHAPE('',$,#11410);
#11342=PRODUCT_DEFINITION_SHAPE('',$,#11411);
#11343=PRODUCT_DEFINITION_SHAPE('',$,#11412);
#11344=PRODUCT_DEFINITION_SHAPE('',$,#11413);
#11345=PRODUCT_DEFINITION_SHAPE('',$,#11414);
#11346=PRODUCT_DEFINITION_SHAPE('',$,#11415);
#11347=PRODUCT_DEFINITION_SHAPE($,$,#160);
#11348=PRODUCT_DEFINITION_SHAPE($,$,#161);
#11349=PRODUCT_DEFINITION_SHAPE($,$,#162);
#11350=PRODUCT_DEFINITION_SHAPE($,$,#163);
#11351=PRODUCT_DEFINITION_SHAPE($,$,#164);
#11352=PRODUCT_DEFINITION_SHAPE($,$,#165);
#11353=PRODUCT_DEFINITION_SHAPE('',$,#11416);
#11354=PRODUCT_DEFINITION_SHAPE('',$,#11417);
#11355=PRODUCT_DEFINITION_SHAPE($,$,#166);
#11356=PRODUCT_DEFINITION_SHAPE($,$,#167);
#11357=PRODUCT_DEFINITION_SHAPE($,$,#168);
#11358=PRODUCT_DEFINITION_SHAPE($,$,#169);
#11359=SHAPE_REPRESENTATION('',(#5453,#6063,#6064,#6065),#11229);
#11360=SHAPE_REPRESENTATION('',(#5454,#5871,#5872,#5873,#5874,#5875,#5876,
#5877,#5878,#5879,#5880,#5881,#5882,#5883,#5884,#5885,#5886,#5887,#5888,
#5889,#5890,#5891,#5892,#5893),#11230);
#11361=SHAPE_REPRESENTATION('',(#5455),#11231);
#11362=SHAPE_REPRESENTATION('',(#5483),#11232);
#11363=SHAPE_REPRESENTATION('',(#5507),#11233);
#11364=SHAPE_REPRESENTATION('',(#5521),#11234);
#11365=SHAPE_REPRESENTATION('',(#5530),#11235);
#11366=SHAPE_REPRESENTATION('',(#5539),#11236);
#11367=SHAPE_REPRESENTATION('',(#5548),#11237);
#11368=SHAPE_REPRESENTATION('',(#5569),#11238);
#11369=SHAPE_REPRESENTATION('',(#5639),#11239);
#11370=SHAPE_REPRESENTATION('',(#5680,#5809,#5810,#5811,#5812,#5813),#11240);
#11371=SHAPE_REPRESENTATION('',(#5681),#11241);
#11372=SHAPE_REPRESENTATION('',(#5701),#11242);
#11373=SHAPE_REPRESENTATION('',(#5721),#11243);
#11374=SHAPE_REPRESENTATION('',(#5738),#11244);
#11375=SHAPE_REPRESENTATION('',(#5792),#11245);
#11376=SHAPE_REPRESENTATION('',(#5814),#11246);
#11377=SHAPE_REPRESENTATION('',(#5838),#11247);
#11378=SHAPE_REPRESENTATION('',(#5862),#11248);
#11379=SHAPE_REPRESENTATION('',(#5894,#6028,#6029,#6030,#6031,#6032,#6033),
#11249);
#11380=SHAPE_REPRESENTATION('',(#5895),#11250);
#11381=SHAPE_REPRESENTATION('',(#5909),#11251);
#11382=SHAPE_REPRESENTATION('',(#5918),#11252);
#11383=SHAPE_REPRESENTATION('',(#5932),#11253);
#11384=SHAPE_REPRESENTATION('',(#5947),#11254);
#11385=SHAPE_REPRESENTATION('',(#6011),#11255);
#11386=SHAPE_REPRESENTATION('',(#6034,#6062),#11256);
#11387=SHAPE_REPRESENTATION('',(#6035),#11257);
#11388=PRODUCT_DEFINITION_CONTEXT('part definition',#11477,'design');
#11389=PRODUCT_DEFINITION('PAT-106',
'PAT-106',#11418,#11388);
#11390=PRODUCT_DEFINITION('Base bearings and spring anchor',
'Base bearings and spring anchor',#11419,#11388);
#11391=PRODUCT_DEFINITION('Ratchet demonstrator base',
'Ratchet demonstrator base',#11420,#11388);
#11392=PRODUCT_DEFINITION('Pawl pivot pedestal','Pawl pivot pedestal',#11421,
#11388);
#11393=PRODUCT_DEFINITION('Pawl pivot pin','Pawl pivot pin',#11422,#11388);
#11394=PRODUCT_DEFINITION('Lower pawl spacer','Lower pawl spacer',#11423,
#11388);
#11395=PRODUCT_DEFINITION('Torsion spring guide','Torsion spring guide',
#11424,#11388);
#11396=PRODUCT_DEFINITION('Spring and pawl keeper',
'Spring and pawl keeper',#11425,#11388);
#11397=PRODUCT_DEFINITION('Fixed spring anchor','Fixed spring anchor',#11426,
#11388);
#11398=PRODUCT_DEFINITION('Pivot pedestal','Pivot pedestal',#11427,#11388);
#11399=PRODUCT_DEFINITION('Pivot cap','Pivot cap',#11428,#11388);
#11400=PRODUCT_DEFINITION('Sealed Ball Bearing - 10 x 30 x 9 mm',
'Sealed Ball Bearing - 10 x 30 x 9 mm',#11429,#11388);
#11401=PRODUCT_DEFINITION('Inner ring','Inner ring',#11430,#11388);
#11402=PRODUCT_DEFINITION('Outer ring','Outer ring',#11431,#11388);
#11403=PRODUCT_DEFINITION('Balls','Balls',#11432,#11388);
#11404=PRODUCT_DEFINITION('Cage','Cage',#11433,#11388);
#11405=PRODUCT_DEFINITION('Seals 2RS','Seals 2RS',#11434,#11388);
#11406=PRODUCT_DEFINITION('M5x14 Cap Screw','M5x14 Cap Screw',#11435,#11388);
#11407=PRODUCT_DEFINITION('M4x10 Cap Screw','M4x10 Cap Screw',#11436,#11388);
#11408=PRODUCT_DEFINITION(
'Torsion Spring - 1.6 mm Wire, 12 mm Coil, 4.75 Turns',
'Torsion Spring - 1.6 mm Wire, 12 mm Coil, 4.75 Turns',#11437,#11388);
#11409=PRODUCT_DEFINITION('Ratchet wheel and spindle',
'Ratchet wheel and spindle',#11438,#11388);
#11410=PRODUCT_DEFINITION('Stepped ratchet spindle',
'Stepped ratchet spindle',#11439,#11388);
#11411=PRODUCT_DEFINITION('Lower race sleeve','Lower race sleeve',#11440,
#11388);
#11412=PRODUCT_DEFINITION('Spindle collar','Spindle collar',#11441,#11388);
#11413=PRODUCT_DEFINITION('M4x4 collar screw','M4x4 collar screw',#11442,
#11388);
#11414=PRODUCT_DEFINITION('Ratchet wheel','Ratchet wheel',#11443,#11388);
#11415=PRODUCT_DEFINITION('Socket Set Screw - M5x8',
'Socket Set Screw - M5x8',#11444,#11388);
#11416=PRODUCT_DEFINITION('Spring-biased pawl','Spring-biased pawl',#11445,
#11388);
#11417=PRODUCT_DEFINITION('Pawl with spring reaction tab',
'Pawl with spring reaction tab',#11446,#11388);
#11418=PRODUCT_DEFINITION_FORMATION('',$,#11479);
#11419=PRODUCT_DEFINITION_FORMATION('',$,#11480);
#11420=PRODUCT_DEFINITION_FORMATION('',$,#11481);
#11421=PRODUCT_DEFINITION_FORMATION('',$,#11482);
#11422=PRODUCT_DEFINITION_FORMATION('',$,#11483);
#11423=PRODUCT_DEFINITION_FORMATION('',$,#11484);
#11424=PRODUCT_DEFINITION_FORMATION('',$,#11485);
#11425=PRODUCT_DEFINITION_FORMATION('',$,#11486);
#11426=PRODUCT_DEFINITION_FORMATION('',$,#11487);
#11427=PRODUCT_DEFINITION_FORMATION('',$,#11488);
#11428=PRODUCT_DEFINITION_FORMATION('',$,#11489);
#11429=PRODUCT_DEFINITION_FORMATION('',$,#11490);
#11430=PRODUCT_DEFINITION_FORMATION('',$,#11491);
#11431=PRODUCT_DEFINITION_FORMATION('',$,#11492);
#11432=PRODUCT_DEFINITION_FORMATION('',$,#11493);
#11433=PRODUCT_DEFINITION_FORMATION('',$,#11494);
#11434=PRODUCT_DEFINITION_FORMATION('',$,#11495);
#11435=PRODUCT_DEFINITION_FORMATION('',$,#11496);
#11436=PRODUCT_DEFINITION_FORMATION('',$,#11497);
#11437=PRODUCT_DEFINITION_FORMATION('',$,#11498);
#11438=PRODUCT_DEFINITION_FORMATION('',$,#11499);
#11439=PRODUCT_DEFINITION_FORMATION('',$,#11500);
#11440=PRODUCT_DEFINITION_FORMATION('',$,#11501);
#11441=PRODUCT_DEFINITION_FORMATION('',$,#11502);
#11442=PRODUCT_DEFINITION_FORMATION('',$,#11503);
#11443=PRODUCT_DEFINITION_FORMATION('',$,#11504);
#11444=PRODUCT_DEFINITION_FORMATION('',$,#11505);
#11445=PRODUCT_DEFINITION_FORMATION('',$,#11506);
#11446=PRODUCT_DEFINITION_FORMATION('',$,#11507);
#11447=PRODUCT_RELATED_PRODUCT_CATEGORY(
'PAT-106','PAT-106',(#11479));
#11448=PRODUCT_RELATED_PRODUCT_CATEGORY(
'Base bearings and spring anchor','Base bearings and spring anchor',(#11480));
#11449=PRODUCT_RELATED_PRODUCT_CATEGORY('Ratchet demonstrator base',
'Ratchet demonstrator base',(#11481));
#11450=PRODUCT_RELATED_PRODUCT_CATEGORY('Pawl pivot pedestal',
'Pawl pivot pedestal',(#11482));
#11451=PRODUCT_RELATED_PRODUCT_CATEGORY('Pawl pivot pin',
'Pawl pivot pin',(#11483));
#11452=PRODUCT_RELATED_PRODUCT_CATEGORY('Lower pawl spacer',
'Lower pawl spacer',(#11484));
#11453=PRODUCT_RELATED_PRODUCT_CATEGORY('Torsion spring guide',
'Torsion spring guide',(#11485));
#11454=PRODUCT_RELATED_PRODUCT_CATEGORY('Spring and pawl keeper',
'Spring and pawl keeper',(#11486));
#11455=PRODUCT_RELATED_PRODUCT_CATEGORY('Fixed spring anchor',
'Fixed spring anchor',(#11487));
#11456=PRODUCT_RELATED_PRODUCT_CATEGORY('Pivot pedestal',
'Pivot pedestal',(#11488));
#11457=PRODUCT_RELATED_PRODUCT_CATEGORY('Pivot cap','Pivot cap',(#11489));
#11458=PRODUCT_RELATED_PRODUCT_CATEGORY(
'Sealed Ball Bearing - 10 x 30 x 9 mm',
'Sealed Ball Bearing - 10 x 30 x 9 mm',(#11490));
#11459=PRODUCT_RELATED_PRODUCT_CATEGORY('Inner ring','Inner ring',(#11491));
#11460=PRODUCT_RELATED_PRODUCT_CATEGORY('Outer ring','Outer ring',(#11492));
#11461=PRODUCT_RELATED_PRODUCT_CATEGORY('Balls','Balls',(#11493));
#11462=PRODUCT_RELATED_PRODUCT_CATEGORY('Cage','Cage',(#11494));
#11463=PRODUCT_RELATED_PRODUCT_CATEGORY('Seals 2RS','Seals 2RS',(#11495));
#11464=PRODUCT_RELATED_PRODUCT_CATEGORY('M5x14 Cap Screw',
'M5x14 Cap Screw',(#11496));
#11465=PRODUCT_RELATED_PRODUCT_CATEGORY('M4x10 Cap Screw',
'M4x10 Cap Screw',(#11497));
#11466=PRODUCT_RELATED_PRODUCT_CATEGORY(
'Torsion Spring - 1.6 mm Wire, 12 mm Coil, 4.75 Turns',
'Torsion Spring - 1.6 mm Wire, 12 mm Coil, 4.75 Turns',(#11498));
#11467=PRODUCT_RELATED_PRODUCT_CATEGORY('Ratchet wheel and spindle',
'Ratchet wheel and spindle',(#11499));
#11468=PRODUCT_RELATED_PRODUCT_CATEGORY('Stepped ratchet spindle',
'Stepped ratchet spindle',(#11500));
#11469=PRODUCT_RELATED_PRODUCT_CATEGORY('Lower race sleeve',
'Lower race sleeve',(#11501));
#11470=PRODUCT_RELATED_PRODUCT_CATEGORY('Spindle collar',
'Spindle collar',(#11502));
#11471=PRODUCT_RELATED_PRODUCT_CATEGORY('M4x4 collar screw',
'M4x4 collar screw',(#11503));
#11472=PRODUCT_RELATED_PRODUCT_CATEGORY('Ratchet wheel','Ratchet wheel',
(#11504));
#11473=PRODUCT_RELATED_PRODUCT_CATEGORY('Socket Set Screw - M5x8',
'Socket Set Screw - M5x8',(#11505));
#11474=PRODUCT_RELATED_PRODUCT_CATEGORY('Spring-biased pawl',
'Spring-biased pawl',(#11506));
#11475=PRODUCT_RELATED_PRODUCT_CATEGORY('Pawl with spring reaction tab',
'Pawl with spring reaction tab',(#11507));
#11476=APPLICATION_PROTOCOL_DEFINITION('international standard',
'automotive_design',2009,#11477);
#11477=APPLICATION_CONTEXT(
'Core Data for Automotive Mechanical Design Process');
#11478=PRODUCT_CONTEXT('part definition',#11477,'mechanical');
#11479=PRODUCT('PAT-106',
'PAT-106',
'PAT-106',(#11478));
#11480=PRODUCT('Base bearings and spring anchor',
'Base bearings and spring anchor','Base bearings and spring anchor',(#11478));
#11481=PRODUCT('Ratchet demonstrator base','Ratchet demonstrator base',
'Ratchet demonstrator base',(#11478));
#11482=PRODUCT('Pawl pivot pedestal','Pawl pivot pedestal',
'Pawl pivot pedestal',(#11478));
#11483=PRODUCT('Pawl pivot pin','Pawl pivot pin','Pawl pivot pin',(#11478));
#11484=PRODUCT('Lower pawl spacer','Lower pawl spacer',
'Lower pawl spacer',(#11478));
#11485=PRODUCT('Torsion spring guide','Torsion spring guide',
'Torsion spring guide',(#11478));
#11486=PRODUCT('Spring and pawl keeper','Spring and pawl keeper',
'Spring and pawl keeper',(#11478));
#11487=PRODUCT('Fixed spring anchor','Fixed spring anchor',
'Fixed spring anchor',(#11478));
#11488=PRODUCT('Pivot pedestal','Pivot pedestal','Pivot pedestal',(#11478));
#11489=PRODUCT('Pivot cap','Pivot cap','Pivot cap',(#11478));
#11490=PRODUCT('Sealed Ball Bearing - 10 x 30 x 9 mm',
'Sealed Ball Bearing - 10 x 30 x 9 mm',
'Sealed Ball Bearing - 10 x 30 x 9 mm',(#11478));
#11491=PRODUCT('Inner ring','Inner ring','Inner ring',(#11478));
#11492=PRODUCT('Outer ring','Outer ring','Outer ring',(#11478));
#11493=PRODUCT('Balls','Balls','Balls',(#11478));
#11494=PRODUCT('Cage','Cage','Cage',(#11478));
#11495=PRODUCT('Seals 2RS','Seals 2RS','Seals 2RS',(#11478));
#11496=PRODUCT('M5x14 Cap Screw','M5x14 Cap Screw','M5x14 Cap Screw',(#11478));
#11497=PRODUCT('M4x10 Cap Screw','M4x10 Cap Screw','M4x10 Cap Screw',(#11478));
#11498=PRODUCT('Torsion Spring - 1.6 mm Wire, 12 mm Coil, 4.75 Turns',
'Torsion Spring - 1.6 mm Wire, 12 mm Coil, 4.75 Turns',
'Torsion Spring - 1.6 mm Wire, 12 mm Coil, 4.75 Turns',(#11478));
#11499=PRODUCT('Ratchet wheel and spindle','Ratchet wheel and spindle',
'Ratchet wheel and spindle',(#11478));
#11500=PRODUCT('Stepped ratchet spindle','Stepped ratchet spindle',
'Stepped ratchet spindle',(#11478));
#11501=PRODUCT('Lower race sleeve','Lower race sleeve',
'Lower race sleeve',(#11478));
#11502=PRODUCT('Spindle collar','Spindle collar','Spindle collar',(#11478));
#11503=PRODUCT('M4x4 collar screw','M4x4 collar screw',
'M4x4 collar screw',(#11478));
#11504=PRODUCT('Ratchet wheel','Ratchet wheel','Ratchet wheel',(#11478));
#11505=PRODUCT('Socket Set Screw - M5x8','Socket Set Screw - M5x8',
'Socket Set Screw - M5x8',(#11478));
#11506=PRODUCT('Spring-biased pawl','Spring-biased pawl',
'Spring-biased pawl',(#11478));
#11507=PRODUCT('Pawl with spring reaction tab',
'Pawl with spring reaction tab','Pawl with spring reaction tab',(#11478));
#11508=PRESENTATION_STYLE_ASSIGNMENT((#11515));
#11509=PRESENTATION_STYLE_ASSIGNMENT((#11516));
#11510=PRESENTATION_STYLE_ASSIGNMENT((#11517));
#11511=PRESENTATION_STYLE_ASSIGNMENT((#11518));
#11512=PRESENTATION_STYLE_ASSIGNMENT((#11519));
#11513=PRESENTATION_STYLE_ASSIGNMENT((#11520));
#11514=PRESENTATION_STYLE_ASSIGNMENT((#11521));
#11515=SURFACE_STYLE_USAGE(.BOTH.,#11522);
#11516=SURFACE_STYLE_USAGE(.BOTH.,#11523);
#11517=SURFACE_STYLE_USAGE(.BOTH.,#11524);
#11518=SURFACE_STYLE_USAGE(.BOTH.,#11525);
#11519=SURFACE_STYLE_USAGE(.BOTH.,#11526);
#11520=SURFACE_STYLE_USAGE(.BOTH.,#11527);
#11521=SURFACE_STYLE_USAGE(.BOTH.,#11528);
#11522=SURFACE_SIDE_STYLE('',(#11529));
#11523=SURFACE_SIDE_STYLE('',(#11530));
#11524=SURFACE_SIDE_STYLE('',(#11531));
#11525=SURFACE_SIDE_STYLE('',(#11532));
#11526=SURFACE_SIDE_STYLE('',(#11533));
#11527=SURFACE_SIDE_STYLE('',(#11534));
#11528=SURFACE_SIDE_STYLE('',(#11535));
#11529=SURFACE_STYLE_FILL_AREA(#11536);
#11530=SURFACE_STYLE_FILL_AREA(#11537);
#11531=SURFACE_STYLE_FILL_AREA(#11538);
#11532=SURFACE_STYLE_FILL_AREA(#11539);
#11533=SURFACE_STYLE_FILL_AREA(#11540);
#11534=SURFACE_STYLE_FILL_AREA(#11541);
#11535=SURFACE_STYLE_FILL_AREA(#11542);
#11536=FILL_AREA_STYLE('Steel - Satin',(#11543));
#11537=FILL_AREA_STYLE('CAD Library Painted - Deep blue',(#11544));
#11538=FILL_AREA_STYLE('CAD Library Painted - Engineering blue',(#11545));
#11539=FILL_AREA_STYLE('CAD Library Painted - Steel gray',(#11546));
#11540=FILL_AREA_STYLE('CAD Library Painted - Off white',(#11547));
#11541=FILL_AREA_STYLE('CAD Library Painted - Graphite',(#11548));
#11542=FILL_AREA_STYLE('CAD Library Painted - Light blue',(#11549));
#11543=FILL_AREA_STYLE_COLOUR('Steel - Satin',#11550);
#11544=FILL_AREA_STYLE_COLOUR('CAD Library Painted - Deep blue',#11551);
#11545=FILL_AREA_STYLE_COLOUR('CAD Library Painted - Engineering blue',
#11552);
#11546=FILL_AREA_STYLE_COLOUR('CAD Library Painted - Steel gray',#11553);
#11547=FILL_AREA_STYLE_COLOUR('CAD Library Painted - Off white',#11554);
#11548=FILL_AREA_STYLE_COLOUR('CAD Library Painted - Graphite',#11555);
#11549=FILL_AREA_STYLE_COLOUR('CAD Library Painted - Light blue',#11556);
#11550=COLOUR_RGB('Steel - Satin',0.627450980392157,0.627450980392157,0.627450980392157);
#11551=COLOUR_RGB('CAD Library Painted - Deep blue',0.0784313725490196,
0.203921568627451,0.349019607843137);
#11552=COLOUR_RGB('CAD Library Painted - Engineering blue',0.12156862745098,
0.356862745098039,0.6);
#11553=COLOUR_RGB('CAD Library Painted - Steel gray',0.592156862745098,
0.631372549019608,0.67843137254902);
#11554=COLOUR_RGB('CAD Library Painted - Off white',0.909803921568627,0.901960784313726,
0.858823529411765);
#11555=COLOUR_RGB('CAD Library Painted - Graphite',0.0980392156862745,0.109803921568627,
0.125490196078431);
#11556=COLOUR_RGB('CAD Library Painted - Light blue',0.286274509803922,
0.552941176470588,0.780392156862745);
#11557=COLOUR_RGB('Dark Blue',0.08,0.2,0.34);
#11558=FILL_AREA_STYLE_COLOUR('',#11557);
#11559=FILL_AREA_STYLE('',(#11558));
#11560=SURFACE_STYLE_FILL_AREA(#11559);
#11561=SURFACE_SIDE_STYLE('',(#11560));
#11562=SURFACE_STYLE_USAGE(.BOTH.,#11561);
#11563=PRESENTATION_STYLE_ASSIGNMENT((#11562));
#11564=COLOUR_RGB('Light Blue',0.38,0.62,0.78);
#11565=FILL_AREA_STYLE_COLOUR('',#11564);
#11566=FILL_AREA_STYLE('',(#11565));
#11567=SURFACE_STYLE_FILL_AREA(#11566);
#11568=SURFACE_SIDE_STYLE('',(#11567));
#11569=SURFACE_STYLE_USAGE(.BOTH.,#11568);
#11570=PRESENTATION_STYLE_ASSIGNMENT((#11569));
#11571=COLOUR_RGB('Sky Blue',0.24,0.69,0.87);
#11572=FILL_AREA_STYLE_COLOUR('',#11571);
#11573=FILL_AREA_STYLE('',(#11572));
#11574=SURFACE_STYLE_FILL_AREA(#11573);
#11575=SURFACE_SIDE_STYLE('',(#11574));
#11576=SURFACE_STYLE_USAGE(.BOTH.,#11575);
#11577=PRESENTATION_STYLE_ASSIGNMENT((#11576));
#11578=COLOUR_RGB('Grey',0.48,0.52,0.57);
#11579=FILL_AREA_STYLE_COLOUR('',#11578);
#11580=FILL_AREA_STYLE('',(#11579));
#11581=SURFACE_STYLE_FILL_AREA(#11580);
#11582=SURFACE_SIDE_STYLE('',(#11581));
#11583=SURFACE_STYLE_USAGE(.BOTH.,#11582);
#11584=PRESENTATION_STYLE_ASSIGNMENT((#11583));
#11585=COLOUR_RGB('Black',0.12,0.14,0.17);
#11586=FILL_AREA_STYLE_COLOUR('',#11585);
#11587=FILL_AREA_STYLE('',(#11586));
#11588=SURFACE_STYLE_FILL_AREA(#11587);
#11589=SURFACE_SIDE_STYLE('',(#11588));
#11590=SURFACE_STYLE_USAGE(.BOTH.,#11589);
#11591=PRESENTATION_STYLE_ASSIGNMENT((#11590));
#11592=COLOUR_RGB('Off White',0.89,0.88,0.83);
#11593=FILL_AREA_STYLE_COLOUR('',#11592);
#11594=FILL_AREA_STYLE('',(#11593));
#11595=SURFACE_STYLE_FILL_AREA(#11594);
#11596=SURFACE_SIDE_STYLE('',(#11595));
#11597=SURFACE_STYLE_USAGE(.BOTH.,#11596);
#11598=PRESENTATION_STYLE_ASSIGNMENT((#11597));
ENDSEC;
END-ISO-10303-21;
